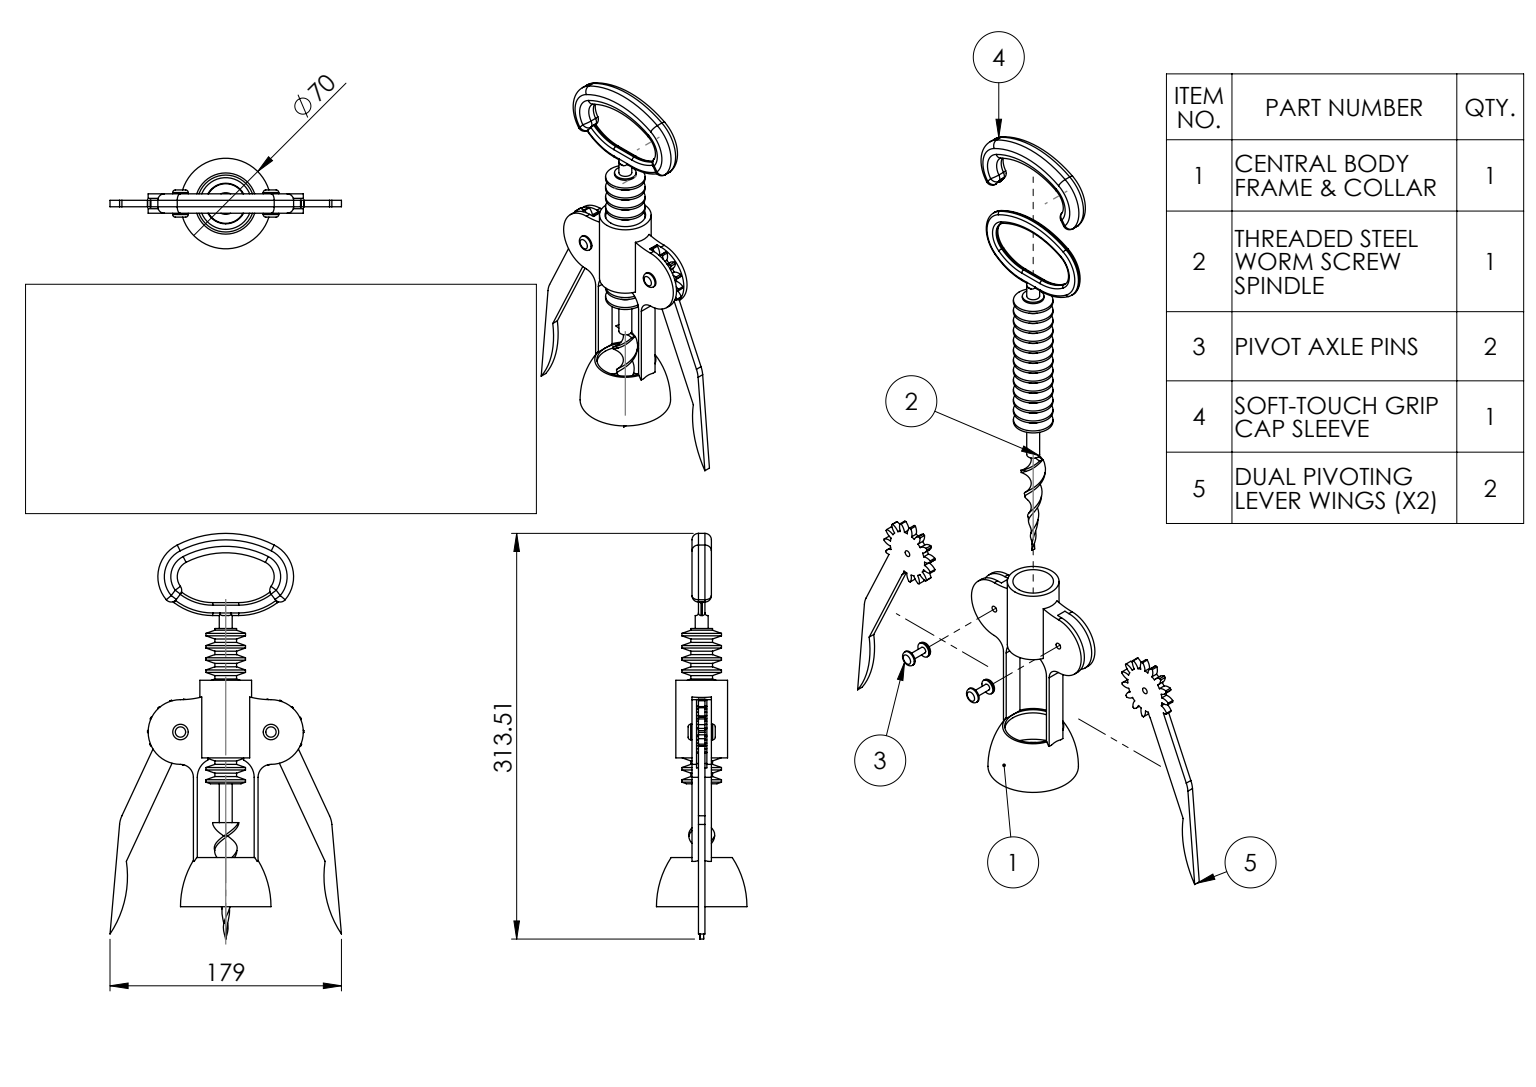
ISO-10303-21;
HEADER;
FILE_DESCRIPTION (('STEP AP214'),
    '1' );
FILE_NAME ('BR-824',
    '2026-10-08T14:03:35',
    ( '' ),
    ( '' ),
    'SwSTEP 2.0',
    'SolidWorks 2026',
    '' );
FILE_SCHEMA (( 'AUTOMOTIVE_DESIGN' ));
ENDSEC;

DATA;
#1 = EDGE_LOOP ( 'NONE', ( #6943, #8347, #5492, #144, #24, #10049, #6379, #1001, #2175, #10989 ) ) ;
#2 = ORIENTED_EDGE ( 'NONE', *, *, #10289, .F. ) ;
#3 = PRODUCT_RELATED_PRODUCT_CATEGORY ( 'part', '', ( #9019 ) ) ;
#4 = VECTOR ( 'NONE', #10867, 1000.000000000000000 ) ;
#5 = CIRCLE ( 'NONE', #8996, 5.999999999999998224 ) ;
#6 = DIRECTION ( 'NONE',  ( 0.9960067511297464593, -0.08927794634716622324, 3.401418580343279473E-17 ) ) ;
#7 = AXIS2_PLACEMENT_3D ( 'NONE', #7492, #359, #1391 ) ;
#8 = ORIENTED_EDGE ( 'NONE', *, *, #7820, .F. ) ;
#9 = ORIENTED_EDGE ( 'NONE', *, *, #2863, .F. ) ;
#10 = CYLINDRICAL_SURFACE ( 'NONE', #6059, 5.000000000000000000 ) ;
#11 = ORIENTED_EDGE ( 'NONE', *, *, #6966, .F. ) ;
#12 = DIRECTION ( 'NONE',  ( -1.000000000000000000, 0.000000000000000000, 0.000000000000000000 ) ) ;
#13 = CARTESIAN_POINT ( 'NONE',  ( 34.99999999999958789, 1.104930248025249758E-13, -2.499999999999999112 ) ) ;
#14 = DIRECTION ( 'NONE',  ( -1.000000000000000000, 0.000000000000000000, 0.000000000000000000 ) ) ;
#15 = CARTESIAN_POINT ( 'NONE',  ( 35.45454545454547457, 140.4866414850956460, 0.5000000000000000000 ) ) ;
#16 = CARTESIAN_POINT ( 'NONE',  ( -12.99553232110413248, 67.62342244460847951, -25.99106464220826851 ) ) ;
#17 = EDGE_CURVE ( 'NONE', #9929, #10530, #4223, .T. ) ;
#18 = VECTOR ( 'NONE', #6174, 1000.000000000000000 ) ;
#19 = CARTESIAN_POINT ( 'NONE',  ( 4.330127018922190985, 92.00000000000000000, -2.500000000000000000 ) ) ;
#20 = CARTESIAN_POINT ( 'NONE',  ( 10.69381717166375623, 25.55944687211528077, 0.000000000000000000 ) ) ;
#21 = ADVANCED_FACE ( 'NONE', ( #11217 ), #12542, .T. ) ;
#22 = ORIENTED_EDGE ( 'NONE', *, *, #10210, .T. ) ;
#23 = AXIS2_PLACEMENT_3D ( 'NONE', #10959, #4438, #5501 ) ;
#24 = ORIENTED_EDGE ( 'NONE', *, *, #1458, .F. ) ;
#25 = EDGE_LOOP ( 'NONE', ( #11281, #8827, #8911, #8959 ) ) ;
#26 = EDGE_CURVE ( 'NONE', #11146, #5183, #4908, .T. ) ;
#27 = EDGE_CURVE ( 'NONE', #5877, #10681, #5933, .T. ) ;
#28 = DIRECTION ( 'NONE',  ( -0.000000000000000000, -0.000000000000000000, -1.000000000000000000 ) ) ;
#29 = AXIS2_PLACEMENT_3D ( 'NONE', #13329, #9153, #677 ) ;
#30 = VERTEX_POINT ( 'NONE', #13473 ) ;
#31 = CARTESIAN_POINT ( 'NONE',  ( 25.00000000000000355, 120.0000000000000284, -0.5000000000000000000 ) ) ;
#32 = CARTESIAN_POINT ( 'NONE',  ( 8.259026987433399469, -87.08508809531834061, -4.189641850005036083 ) ) ;
#33 = CIRCLE ( 'NONE', #4726, 10.00000000000000178 ) ;
#34 = DIRECTION ( 'NONE',  ( 0.9960067511297463483, -0.08927794634716618161, 4.818676322152979407E-17 ) ) ;
#35 = CIRCLE ( 'NONE', #10337, 25.00000000000000711 ) ;
#36 = CARTESIAN_POINT ( 'NONE',  ( -12.99579180576517246, 64.08350967699263379, -3.310582014804570635E-15 ) ) ;
#37 = DIRECTION ( 'NONE',  ( -2.797435172181481150E-17, 1.000000000000000000, -1.765856845898762549E-18 ) ) ;
#38 = CARTESIAN_POINT ( 'NONE',  ( -4.250272934615508369, -76.81818181818270830, -9.136824450690360422 ) ) ;
#39 = DIRECTION ( 'NONE',  ( 1.000000000000000000, 0.000000000000000000, 0.000000000000000000 ) ) ;
#40 = DIRECTION ( 'NONE',  ( 1.000000000000000000, 8.163404592832038896E-16, 0.000000000000000000 ) ) ;
#41 = B_SPLINE_CURVE_WITH_KNOTS ( 'NONE', 3,
 ( #7096, #11371, #11645, #793, #10657, #9414, #8218, #1840, #4203, #6320, #13730, #12506, #2044, #8486, #3154, #2892, #3943, #7162, #10396, #1973, #13588, #10461, #11447, #12783, #5330, #6125, #4075, #12585, #8357, #859, #3030, #10593, #5066, #6254, #12653, #997, #11713, #7433, #2104, #9347, #5125, #1907, #13657, #4005, #8288, #6388, #5261, #1067, #2965, #7233, #7301, #11516, #11582, #3091, #9550, #6196, #8427, #10523, #931, #13858, #5196, #9484, #13791, #4141, #12715, #7359, #12055, #6584, #8618, #1398, #12856, #9746, #158, #7499, #6454, #13067, #1133, #3221, #9677, #5393, #292, #12926, #10918, #4547, #2170, #6728, #3289, #81, #6655, #1321, #7637, #10717, #10997, #7564, #11781, #2240, #8759, #3423, #4335, #11846, #8825, #2370, #2303, #8688, #6525, #10783, #4276, #9612 ),
 .UNSPECIFIED., .F., .F.,
 ( 4, 2, 2, 2, 2, 2, 2, 2, 2, 2, 2, 2, 2, 2, 2, 2, 2, 2, 2, 2, 2, 2, 2, 2, 2, 2, 2, 2, 2, 2, 2, 2, 2, 2, 2, 2, 2, 2, 2, 2, 2, 2, 2, 2, 2, 2, 2, 2, 2, 2, 2, 2, 2, 4 ),
 ( 1.115175723065530429E-16, 0.0007940898450324740008, 0.001588179690064836329, 0.003176359380129561202, 0.004764539070194286074, 0.006352718760259011381, 0.007940898450323734953, 0.009529078140388459392, 0.01111725783045318383, 0.01270543752051791001, 0.01588179690064744215, 0.01905815628077697083, 0.02223451566090650297, 0.02382269535097126731, 0.02541087504103603512, 0.02858723442116564359, 0.03017541411123044609, 0.03176359380129525206, 0.03493995318142493339, 0.03652813287148980875, 0.03811631256155468411, 0.04129267194168446953, 0.04288085163174937264, 0.04446903132181426188, 0.04764539070194404730, 0.04923357039200896429, 0.05082175008207386740, 0.05399810946220368751, 0.05717446884233351456, 0.05876264853239842462, 0.06035082822246332079, 0.06352718760259316866, 0.06511536729265808565, 0.06670354698272301652, 0.06829172667278794739, 0.06987990636285287827, 0.07305626574298272613, 0.07464444543304765700, 0.07623262512311257399, 0.07782080481317750487, 0.07940898450324243574, 0.08258534388337231136, 0.08417352357343724223, 0.08576170326350217310, 0.08734988295356710397, 0.08893806264363202096, 0.09211442202376185495, 0.09370260171382675807, 0.09529078140389167506, 0.09687896109395660593, 0.09846714078402152293, 0.1000553204740864260, 0.1008494103191188984, 0.1016435001641513708 ),
 .UNSPECIFIED. ) ;
#42 = VERTEX_POINT ( 'NONE', #3602 ) ;
#43 = EDGE_CURVE ( 'NONE', #8596, #8398, #2943, .T. ) ;
#44 = AXIS2_PLACEMENT_3D ( 'NONE', #13672, #4217, #12871 ) ;
#45 = AXIS2_PLACEMENT_3D ( 'NONE', #8376, #5215, #8445 ) ;
#46 = FACE_OUTER_BOUND ( 'NONE', #6458, .T. ) ;
#47 = EDGE_LOOP ( 'NONE', ( #4618, #2570, #12122, #10874, #7639, #5291, #7255 ) ) ;
#48 = ORIENTED_EDGE ( 'NONE', *, *, #13831, .T. ) ;
#49 = CARTESIAN_POINT ( 'NONE',  ( 2.406219558548489190E-16, -8.601520358636511432, 1.518905361043589440E-17 ) ) ;
#50 = ORIENTED_EDGE ( 'NONE', *, *, #9118, .T. ) ;
#51 = DIRECTION ( 'NONE',  ( 0.9960067511297463483, -0.08927794634716618161, 4.818676322152979407E-17 ) ) ;
#52 = DIRECTION ( 'NONE',  ( -2.797435172181481150E-17, 1.000000000000000000, -1.765856845898762549E-18 ) ) ;
#53 = CARTESIAN_POINT ( 'NONE',  ( 1.800977217354326365, -65.63636364725842043, 1.354836293522729163 ) ) ;
#54 = CIRCLE ( 'NONE', #4755, 69.24999999999975842 ) ;
#55 = B_SPLINE_CURVE_WITH_KNOTS ( 'NONE', 3,
 ( #12024, #7964, #3604, #11191, #2412, #1580, #5937, #3460, #13327, #5788, #331, #6692, #3526, #3678, #4586, #9152 ),
 .UNSPECIFIED., .F., .F.,
 ( 4, 2, 2, 2, 2, 2, 2, 4 ),
 ( 1.967444805616585729E-07, 0.0004077652619395022980, 0.0008153337793984429286, 0.001630470814316324190, 0.002038039331775264550, 0.002445607849234205343, 0.002853176366693145703, 0.003260744884152086496 ),
 .UNSPECIFIED. ) ;
#56 = FACE_OUTER_BOUND ( 'NONE', #8177, .T. ) ;
#57 = CARTESIAN_POINT ( 'NONE',  ( -8.385254915620292238, 24.75422479069652937, -16.77050983124059158 ) ) ;
#58 = CARTESIAN_POINT ( 'NONE',  ( -15.29705854078140348, -29.33764382806072746, 30.59411708156278920 ) ) ;
#59 = CARTESIAN_POINT ( 'NONE',  ( -2.079471018873752021E-15, 74.33491362204294717, -1.312648161087776599E-16 ) ) ;
#60 = DIRECTION ( 'NONE',  ( -1.000000000000000000, 0.000000000000000000, 0.000000000000000000 ) ) ;
#61 = EDGE_CURVE ( 'NONE', #7055, #3214, #4012, .T. ) ;
#62 = EDGE_LOOP ( 'NONE', ( #12490, #5333, #1562, #12326 ) ) ;
#63 = ORIENTED_EDGE ( 'NONE', *, *, #3775, .F. ) ;
#64 = CARTESIAN_POINT ( 'NONE',  ( -10.69381717166375800, 53.83378072214353693, -1.499740397452121781E-15 ) ) ;
#65 = LINE ( 'NONE', #1951, #2569 ) ;
#66 = CARTESIAN_POINT ( 'NONE',  ( 34.99999999999958789, 1.104930248025249758E-13, -2.499999999999999112 ) ) ;
#67 = CARTESIAN_POINT ( 'NONE',  ( -15.18222645069203125, -100.0000000000000000, -4.000000000000000000 ) ) ;
#68 = DIRECTION ( 'NONE',  ( -6.158143864569485777E-17, -2.736152283717910599E-16, 1.000000000000000000 ) ) ;
#69 = ORIENTED_EDGE ( 'NONE', *, *, #3097, .T. ) ;
#70 = ORIENTED_EDGE ( 'NONE', *, *, #7148, .F. ) ;
#71 = ADVANCED_FACE ( 'NONE', ( #7311 ), #13694, .F. ) ;
#72 = ORIENTED_EDGE ( 'NONE', *, *, #13139, .F. ) ;
#73 = ORIENTED_EDGE ( 'NONE', *, *, #707, .T. ) ;
#74 = ORIENTED_EDGE ( 'NONE', *, *, #8494, .F. ) ;
#75 = CARTESIAN_POINT ( 'NONE',  ( -34.99999999999999289, -97.00000000000000000, -7.500000000000000000 ) ) ;
#76 = AXIS2_PLACEMENT_3D ( 'NONE', #13638, #11239, #6171 ) ;
#77 = FACE_BOUND ( 'NONE', #7085, .T. ) ;
#78 = CARTESIAN_POINT ( 'NONE',  ( 0.3899450390716444614, -79.59552052770862929, -10.11716208056824762 ) ) ;
#79 = DIRECTION ( 'NONE',  ( -1.000000000000000000, 0.000000000000000000, 0.000000000000000000 ) ) ;
#80 = CARTESIAN_POINT ( 'NONE',  ( 3.915931169992960648, 90.55292468037850995, -3.111431273932147246 ) ) ;
#81 = CARTESIAN_POINT ( 'NONE',  ( -7.912770636739809405, -89.29698991853884138, 4.227864033747772865 ) ) ;
#82 = CARTESIAN_POINT ( 'NONE',  ( 25.00000000000001776, -100.0000000000000000, -5.046127144242417373 ) ) ;
#83 = EDGE_LOOP ( 'NONE', ( #9533, #5553, #4896, #10180 ) ) ;
#84 = ORIENTED_EDGE ( 'NONE', *, *, #10476, .F. ) ;
#85 = ORIENTED_EDGE ( 'NONE', *, *, #10554, .F. ) ;
#86 = AXIS2_PLACEMENT_3D ( 'NONE', #6886, #3650, #3573 ) ;
#87 = AXIS2_PLACEMENT_3D ( 'NONE', #13479, #2566, #7966 ) ;
#88 = ADVANCED_FACE ( 'NONE', ( #12662 ), #10538, .T. ) ;
#89 = DIRECTION ( 'NONE',  ( 6.158143864569485777E-17, 2.736152283717910599E-16, -1.000000000000000000 ) ) ;
#90 = EDGE_CURVE ( 'NONE', #3108, #8314, #5574, .T. ) ;
#91 = ORIENTED_EDGE ( 'NONE', *, *, #2062, .T. ) ;
#92 = DIRECTION ( 'NONE',  ( -0.8735848310779960046, 0.4866719047884612293, 9.637352644305955116E-17 ) ) ;
#93 = AXIS2_PLACEMENT_3D ( 'NONE', #1306, #12036, #9868 ) ;
#94 = DIRECTION ( 'NONE',  ( 0.000000000000000000, 0.000000000000000000, 1.000000000000000000 ) ) ;
#95 = CARTESIAN_POINT ( 'NONE',  ( 21.12690199240172007, 12.61198448588842425, -2.499999999999996447 ) ) ;
#96 = CARTESIAN_POINT ( 'NONE',  ( -2.905947830705728041, -133.0909090909398458, 2.158723819798283206 ) ) ;
#97 = CARTESIAN_POINT ( 'NONE',  ( -26.79177319725820894, -26.24642857144861807, -4.000000000000000000 ) ) ;
#98 = CARTESIAN_POINT ( 'NONE',  ( -60.00000000000001421, -4.286263797015736496E-15, 7.500000000000000000 ) ) ;
#99 = EDGE_CURVE ( 'NONE', #9883, #11270, #7176, .T. ) ;
#100 = CARTESIAN_POINT ( 'NONE',  ( 1.824130267506742786, -166.5454545852088017, -2.249022964541941061 ) ) ;
#101 = EDGE_CURVE ( 'NONE', #11832, #6555, #12065, .T. ) ;
#102 = CARTESIAN_POINT ( 'NONE',  ( -1.416598489609734557, -78.09090909090909349, -10.12631592825915838 ) ) ;
#103 = B_SPLINE_CURVE_WITH_KNOTS ( 'NONE', 3,
 ( #9323, #12223, #13300, #13225 ),
 .UNSPECIFIED., .F., .F.,
 ( 4, 4 ),
 ( 0.000000000000000000, 1.000000000000000000 ),
 .UNSPECIFIED. ) ;
#104 = CARTESIAN_POINT ( 'NONE',  ( 35.00000000000000000, 4.286263797015736496E-15, 7.500000000000000000 ) ) ;
#105 = LINE ( 'NONE', #1342, #981 ) ;
#106 = VECTOR ( 'NONE', #4632, 1000.000000000000000 ) ;
#107 = ORIENTED_EDGE ( 'NONE', *, *, #7623, .T. ) ;
#108 = CARTESIAN_POINT ( 'NONE',  ( 39.99999999999999289, 120.0000000000000142, -0.5000000000000000000 ) ) ;
#109 = CARTESIAN_POINT ( 'NONE',  ( 43.14708730495711819, 24.16350488746832781, 2.500000000000007105 ) ) ;
#110 = ORIENTED_EDGE ( 'NONE', *, *, #13403, .F. ) ;
#111 = CIRCLE ( 'NONE', #7943, 15.29705854078139460 ) ;
#112 = ADVANCED_FACE ( 'NONE', ( #12595 ), #4281, .T. ) ;
#113 = LINE ( 'NONE', #13095, #3464 ) ;
#114 = EDGE_CURVE ( 'NONE', #2716, #3638, #13476, .T. ) ;
#115 = DIRECTION ( 'NONE',  ( 0.000000000000000000, 0.000000000000000000, 1.000000000000000000 ) ) ;
#116 = ORIENTED_EDGE ( 'NONE', *, *, #6600, .T. ) ;
#117 = AXIS2_PLACEMENT_3D ( 'NONE', #10882, #1230, #12167 ) ;
#118 = CARTESIAN_POINT ( 'NONE',  ( 8.385254915620292238, 90.00000000000000000, 8.679704431140114636E-16 ) ) ;
#119 = CARTESIAN_POINT ( 'NONE',  ( -15.29705854078139637, 74.33491362204294717, -1.312648161087776599E-16 ) ) ;
#120 = CARTESIAN_POINT ( 'NONE',  ( -8.385254915620295790, 3.280056672672170492, 16.77050983124058448 ) ) ;
#121 = AXIS2_PLACEMENT_3D ( 'NONE', #813, #875, #8370 ) ;
#122 = EDGE_CURVE ( 'NONE', #8713, #9553, #6328, .T. ) ;
#123 = CARTESIAN_POINT ( 'NONE',  ( 35.00000000000009237, 91.25000000000046896, 4.000000000000000000 ) ) ;
#124 = EDGE_CURVE ( 'NONE', #4194, #10453, #1869, .T. ) ;
#125 = CARTESIAN_POINT ( 'NONE',  ( -12.99579180576517246, -20.73949187309215247, -1.518279536322449159E-15 ) ) ;
#126 = CARTESIAN_POINT ( 'NONE',  ( -8.385254915620294014, 12.70483462268159869, -2.089658196149648066E-15 ) ) ;
#127 = CYLINDRICAL_SURFACE ( 'NONE', #2611, 18.74900000001875000 ) ;
#128 = CYLINDRICAL_SURFACE ( 'NONE', #1187, 18.74900000001875000 ) ;
#129 = CARTESIAN_POINT ( 'NONE',  ( -35.00000000000000000, -4.286263797015736496E-15, 4.000000000000000000 ) ) ;
#130 = AXIS2_PLACEMENT_3D ( 'NONE', #4348, #7713, #2181 ) ;
#131 = VERTEX_POINT ( 'NONE', #11545 ) ;
#132 = AXIS2_PLACEMENT_3D ( 'NONE', #2558, #4657, #7593 ) ;
#133 = EDGE_CURVE ( 'NONE', #3737, #3625, #5810, .T. ) ;
#134 = ADVANCED_FACE ( 'NONE', ( #1030, #12741 ), #7261, .F. ) ;
#135 = ORIENTED_EDGE ( 'NONE', *, *, #9456, .T. ) ;
#136 = ORIENTED_EDGE ( 'NONE', *, *, #744, .F. ) ;
#137 = AXIS2_PLACEMENT_3D ( 'NONE', #11805, #13167, #2478 ) ;
#138 = CARTESIAN_POINT ( 'NONE',  ( -49.99999999999999289, 120.0000000000000142, -0.5000000000000000000 ) ) ;
#139 = EDGE_CURVE ( 'NONE', #6890, #1913, #9510, .T. ) ;
#140 = FACE_OUTER_BOUND ( 'NONE', #958, .T. ) ;
#141 = VECTOR ( 'NONE', #5529, 1000.000000000000000 ) ;
#142 = CARTESIAN_POINT ( 'NONE',  ( -35.00000000000000000, 25.00000000000000000, -4.000000000000000000 ) ) ;
#143 = DIRECTION ( 'NONE',  ( -2.797435172181481150E-17, 1.000000000000000000, -1.765856845898762549E-18 ) ) ;
#144 = ORIENTED_EDGE ( 'NONE', *, *, #11064, .F. ) ;
#145 = EDGE_LOOP ( 'NONE', ( #4394, #1634, #10776, #9029 ) ) ;
#146 = AXIS2_PLACEMENT_3D ( 'NONE', #3923, #12417, #8205 ) ;
#147 = CIRCLE ( 'NONE', #5069, 5.000000000000000000 ) ;
#148 = ORIENTED_EDGE ( 'NONE', *, *, #400, .T. ) ;
#149 = VERTEX_POINT ( 'NONE', #5637 ) ;
#150 = CARTESIAN_POINT ( 'NONE',  ( 15.29705854078138927, 55.48535772202409078, 1.773704474924340737E-15 ) ) ;
#151 = ORIENTED_EDGE ( 'NONE', *, *, #13444, .T. ) ;
#152 = DIRECTION ( 'NONE',  ( 1.000000000000000000, 0.000000000000000000, 0.000000000000000000 ) ) ;
#153 = CARTESIAN_POINT ( 'NONE',  ( 43.29712336220986657, 19.44704974301885159, -2.499999999999993783 ) ) ;
#154 = AXIS2_PLACEMENT_3D ( 'NONE', #13891, #2740, #9326 ) ;
#155 =( LENGTH_UNIT ( ) NAMED_UNIT ( * ) SI_UNIT ( .MILLI., .METRE. ) );
#156 = DIRECTION ( 'NONE',  ( -2.797435172181481150E-17, 1.000000000000000000, -1.765856845898762549E-18 ) ) ;
#157 = DIRECTION ( 'NONE',  ( -0.6001121574638169642, 0.7999158696163758409, 1.927470528861191270E-16 ) ) ;
#158 = CARTESIAN_POINT ( 'NONE',  ( -5.529376117763302290, -98.63915323273988633, -5.578400940830572807 ) ) ;
#159 = B_SPLINE_CURVE_WITH_KNOTS ( 'NONE', 3,
 ( #12320, #4952, #9234, #13548 ),
 .UNSPECIFIED., .F., .F.,
 ( 4, 4 ),
 ( 0.000000000000000000, 1.000000000000000000 ),
 .UNSPECIFIED. ) ;
#160 = CYLINDRICAL_SURFACE ( 'NONE', #3931, 25.50000000002549783 ) ;
#161 = ORIENTED_EDGE ( 'NONE', *, *, #4188, .T. ) ;
#162 = ORIENTED_EDGE ( 'NONE', *, *, #8775, .F. ) ;
#163 = ORIENTED_EDGE ( 'NONE', *, *, #556, .F. ) ;
#164 = CIRCLE ( 'NONE', #12478, 50.00000000000001421 ) ;
#165 = FACE_OUTER_BOUND ( 'NONE', #5586, .T. ) ;
#166 = CARTESIAN_POINT ( 'NONE',  ( 31.81818181818183433, 133.3608531424536920, 2.500000000000000000 ) ) ;
#167 = ORIENTED_EDGE ( 'NONE', *, *, #10705, .F. ) ;
#168 = CYLINDRICAL_SURFACE ( 'NONE', #12862, 25.50000000002549783 ) ;
#169 = CARTESIAN_POINT ( 'NONE',  ( -15.29705854078138927, 19.67281349139174296, -3.473937238186366113E-17 ) ) ;
#170 = DIRECTION ( 'NONE',  ( -6.158143864569485777E-17, -2.736152283717910599E-16, 1.000000000000000000 ) ) ;
#171 = DIRECTION ( 'NONE',  ( 0.000000000000000000, 0.000000000000000000, 1.000000000000000000 ) ) ;
#172 = CYLINDRICAL_SURFACE ( 'NONE', #13260, 80.00000000000001421 ) ;
#173 = CARTESIAN_POINT ( 'NONE',  ( -9.456627357064087747, -73.18181818181821541, -3.908318357316046487 ) ) ;
#174 = CYLINDRICAL_SURFACE ( 'NONE', #4487, 2.500000000000002220 ) ;
#175 = CARTESIAN_POINT ( 'NONE',  ( 53.63671053572210923, -2.048907369402451106, 2.500000000000000444 ) ) ;
#176 = ADVANCED_FACE ( 'NONE', ( #6620 ), #9921, .T. ) ;
#177 = ORIENTED_EDGE ( 'NONE', *, *, #6787, .T. ) ;
#178 = DIRECTION ( 'NONE',  ( 1.000000000000000000, 0.000000000000000000, 0.000000000000000000 ) ) ;
#179 = ORIENTED_EDGE ( 'NONE', *, *, #7625, .T. ) ;
#180 = CARTESIAN_POINT ( 'NONE',  ( -2.517691654963332357E-15, 90.00000000000000000, -1.589271161308885878E-16 ) ) ;
#181 = DIRECTION ( 'NONE',  ( -0.000000000000000000, -0.000000000000000000, -1.000000000000000000 ) ) ;
#182 = VERTEX_POINT ( 'NONE', #256 ) ;
#183 = CARTESIAN_POINT ( 'NONE',  ( -12.99579180576516535, 7.534841976936128560, -1.618136388307047266E-15 ) ) ;
#184 = CARTESIAN_POINT ( 'NONE',  ( -35.00000000000012079, 91.25000000000045475, -7.500000000000000000 ) ) ;
#185 = CARTESIAN_POINT ( 'NONE',  ( 12.99579180576516713, 73.50828762700209040, 0.000000000000000000 ) ) ;
#186 = CARTESIAN_POINT ( 'NONE',  ( 41.86252833142972918, 24.55922850786694056, 2.500000000000007105 ) ) ;
#187 = DIRECTION ( 'NONE',  ( -1.000000000000000000, 0.000000000000000000, 0.000000000000000000 ) ) ;
#188 = FACE_OUTER_BOUND ( 'NONE', #11939, .T. ) ;
#189 = DIRECTION ( 'NONE',  ( -6.158143864569485777E-17, -2.736152283717910599E-16, 1.000000000000000000 ) ) ;
#190 = EDGE_CURVE ( 'NONE', #2348, #11393, #10077, .T. ) ;
#191 = DIRECTION ( 'NONE',  ( -2.797435172181481150E-17, 1.000000000000000000, -1.765856845898762549E-18 ) ) ;
#192 = ADVANCED_FACE ( 'NONE', ( #6688 ), #1879, .T. ) ;
#193 = ADVANCED_FACE ( 'NONE', ( #9782 ), #3762, .T. ) ;
#194 = CARTESIAN_POINT ( 'NONE',  ( 35.00000000000000000, 4.286263797015736496E-15, 4.000000000000000000 ) ) ;
#195 = EDGE_LOOP ( 'NONE', ( #3953, #4577 ) ) ;
#196 = CARTESIAN_POINT ( 'NONE',  ( 0.000000000000000000, 71.01020514433645303, 7.500000000000000000 ) ) ;
#197 = ADVANCED_FACE ( 'NONE', ( #5497 ), #1357, .T. ) ;
#198 = ADVANCED_FACE ( 'NONE', ( #8588 ), #2424, .T. ) ;
#199 = AXIS2_PLACEMENT_3D ( 'NONE', #10505, #5245, #13714 ) ;
#200 = ORIENTED_EDGE ( 'NONE', *, *, #12255, .T. ) ;
#201 = AXIS2_PLACEMENT_3D ( 'NONE', #5042, #6172, #12757 ) ;
#202 = ORIENTED_EDGE ( 'NONE', *, *, #10624, .T. ) ;
#203 = CARTESIAN_POINT ( 'NONE',  ( 80.29381926039658879, -64.72749139719506672, -2.500000000000000000 ) ) ;
#204 = FACE_OUTER_BOUND ( 'NONE', #4519, .T. ) ;
#205 = PLANE ( 'NONE',  #6332 ) ;
#206 = AXIS2_PLACEMENT_3D ( 'NONE', #6163, #5168, #5231 ) ;
#207 = EDGE_CURVE ( 'NONE', #13779, #9777, #1115, .T. ) ;
#208 = DIRECTION ( 'NONE',  ( 1.000000000000000000, 0.000000000000000000, -0.000000000000000000 ) ) ;
#209 = EDGE_LOOP ( 'NONE', ( #5485, #10650, #4189, #10104 ) ) ;
#210 = ORIENTED_EDGE ( 'NONE', *, *, #10551, .T. ) ;
#211 = EDGE_CURVE ( 'NONE', #2222, #2825, #5653, .T. ) ;
#212 = CARTESIAN_POINT ( 'NONE',  ( -13.79311422413708499, -100.0000000000000000, 7.500000000000000000 ) ) ;
#213 = EDGE_LOOP ( 'NONE', ( #12461, #12603, #11855, #6788 ) ) ;
#214 = VERTEX_POINT ( 'NONE', #5795 ) ;
#215 = DIRECTION ( 'NONE',  ( -2.797435172181481150E-17, 1.000000000000000000, -1.765856845898762549E-18 ) ) ;
#216 = ORIENTED_EDGE ( 'NONE', *, *, #1663, .T. ) ;
#217 = CARTESIAN_POINT ( 'NONE',  ( -1.868594470333698657E-15, 66.79670324143890525, -1.179534157023628988E-16 ) ) ;
#218 = DIRECTION ( 'NONE',  ( -0.000000000000000000, -0.000000000000000000, -1.000000000000000000 ) ) ;
#219 = CYLINDRICAL_SURFACE ( 'NONE', #7081, 8.385254915620292238 ) ;
#220 = DIRECTION ( 'NONE',  ( 0.1928999275155749149, 0.9812184353977894125, 2.775705599192072226E-16 ) ) ;
#221 = CARTESIAN_POINT ( 'NONE',  ( -15.29705854078139282, -29.33764382806072746, -30.59411708156279630 ) ) ;
#222 = DIRECTION ( 'NONE',  ( 6.158143864569485777E-17, 2.736152283717910599E-16, -1.000000000000000000 ) ) ;
#223 = EDGE_LOOP ( 'NONE', ( #1388, #322, #1636, #10853 ) ) ;
#224 = AXIS2_PLACEMENT_3D ( 'NONE', #10271, #2564, #8106 ) ;
#225 = ORIENTED_EDGE ( 'NONE', *, *, #6865, .T. ) ;
#226 = ORIENTED_EDGE ( 'NONE', *, *, #7270, .T. ) ;
#227 = AXIS2_PLACEMENT_3D ( 'NONE', #6286, #961, #5222 ) ;
#228 = FACE_OUTER_BOUND ( 'NONE', #3050, .T. ) ;
#229 = CARTESIAN_POINT ( 'NONE',  ( -0.9875499244693202172, -80.00464164737402939, 10.06307371418729701 ) ) ;
#230 = ORIENTED_EDGE ( 'NONE', *, *, #3262, .F. ) ;
#231 = DIRECTION ( 'NONE',  ( -1.224646799147353207E-16, 1.000000000000000000, 0.000000000000000000 ) ) ;
#232 = CARTESIAN_POINT ( 'NONE',  ( -25.00000000000000355, 120.0000000000000284, 0.5000000000000000000 ) ) ;
#233 = CARTESIAN_POINT ( 'NONE',  ( -15.29705854078139637, 0.8232575913728885642, -1.453755053663958216E-18 ) ) ;
#234 = DIRECTION ( 'NONE',  ( -1.000000000000000000, 0.000000000000000000, 0.000000000000000000 ) ) ;
#235 = CARTESIAN_POINT ( 'NONE',  ( -2.866821506922881722E-16, 10.24803554138234496, -1.809656371776380929E-17 ) ) ;
#236 = CARTESIAN_POINT ( 'NONE',  ( 1.713057075396043238, -163.8787878899150030, 2.641018403436653728 ) ) ;
#237 = VECTOR ( 'NONE', #1930, 1000.000000000000000 ) ;
#238 = CARTESIAN_POINT ( 'NONE',  ( 15.29705854078138927, 46.06057977201469100, 1.790347283588440388E-15 ) ) ;
#239 = CIRCLE ( 'NONE', #906, 9.000000000008999024 ) ;
#240 = CARTESIAN_POINT ( 'NONE',  ( 18.54049621773915746, -20.00000000000000000, -7.500000000000000000 ) ) ;
#241 = FILL_AREA_STYLE ('',( #9833 ) ) ;
#242 = ORIENTED_EDGE ( 'NONE', *, *, #7205, .T. ) ;
#243 = CYLINDRICAL_SURFACE ( 'NONE', #12092, 8.385254915620295790 ) ;
#244 = CARTESIAN_POINT ( 'NONE',  ( 0.4999999999999966693, 79.99058638175036151, -2.499999999999982236 ) ) ;
#245 = AXIS2_PLACEMENT_3D ( 'NONE', #10275, #9294, #13478 ) ;
#246 = ORIENTED_EDGE ( 'NONE', *, *, #1045, .F. ) ;
#247 = CIRCLE ( 'NONE', #2028, 15.29705854078138572 ) ;
#248 = AXIS2_PLACEMENT_3D ( 'NONE', #3744, #8028, #12308 ) ;
#249 = DIRECTION ( 'NONE',  ( 0.000000000000000000, -1.000000000000000000, 0.000000000000000000 ) ) ;
#250 = CARTESIAN_POINT ( 'NONE',  ( 36.36363636363638108, 142.2680885707561629, 2.500000000000000000 ) ) ;
#251 = ORIENTED_EDGE ( 'NONE', *, *, #10047, .F. ) ;
#252 = DIRECTION ( 'NONE',  ( -2.797435172181481150E-17, 1.000000000000000000, -1.765856845898762549E-18 ) ) ;
#253 = ORIENTED_EDGE ( 'NONE', *, *, #309, .F. ) ;
#254 = CARTESIAN_POINT ( 'NONE',  ( 51.25836974494252019, 19.64472991003004054, 6.505213034913026604E-15 ) ) ;
#255 = EDGE_CURVE ( 'NONE', #10763, #2744, #8961, .T. ) ;
#256 = CARTESIAN_POINT ( 'NONE',  ( 23.90723890023449627, -15.11541108221136476, -2.500000000000003553 ) ) ;
#257 = DIRECTION ( 'NONE',  ( -0.000000000000000000, -0.000000000000000000, 1.000000000000000000 ) ) ;
#258 = AXIS2_PLACEMENT_3D ( 'NONE', #3303, #12076, #6668 ) ;
#259 = CARTESIAN_POINT ( 'NONE',  ( -12.99579180576516713, -1.889935973073298525, -1.584850770978847568E-15 ) ) ;
#260 = DIRECTION ( 'NONE',  ( 0.000000000000000000, 0.000000000000000000, 1.000000000000000000 ) ) ;
#261 = FACE_OUTER_BOUND ( 'NONE', #11503, .T. ) ;
#262 = DIRECTION ( 'NONE',  ( -1.000000000000000000, -5.171946152600902986E-17, 0.000000000000000000 ) ) ;
#263 = AXIS2_PLACEMENT_3D ( 'NONE', #6259, #865, #11653 ) ;
#264 = B_SPLINE_CURVE_WITH_KNOTS ( 'NONE', 3,
 ( #3142, #782, #3995, #11363 ),
 .UNSPECIFIED., .F., .F.,
 ( 4, 4 ),
 ( 0.000000000000000000, 1.000000000000000000 ),
 .UNSPECIFIED. ) ;
#265 = ORIENTED_EDGE ( 'NONE', *, *, #867, .T. ) ;
#266 = ORIENTED_EDGE ( 'NONE', *, *, #11663, .F. ) ;
#267 = LINE ( 'NONE', #5318, #5455 ) ;
#268 = CIRCLE ( 'NONE', #8110, 14.99999999999998934 ) ;
#269 = EDGE_CURVE ( 'NONE', #10258, #13109, #10073, .T. ) ;
#270 = PRODUCT_CONTEXT ( 'NONE', #3147, 'mechanical' ) ;
#271 = EDGE_CURVE ( 'NONE', #8931, #12042, #8495, .T. ) ;
#272 = ORIENTED_EDGE ( 'NONE', *, *, #8857, .F. ) ;
#273 = CARTESIAN_POINT ( 'NONE',  ( 35.22727272727274794, 140.0412797136805523, 2.499999999999999556 ) ) ;
#274 = CARTESIAN_POINT ( 'NONE',  ( -12.99553232110413781, 39.34908859458022334, -1.730463420974848368E-15 ) ) ;
#275 = EDGE_CURVE ( 'NONE', #4145, #2418, #159, .T. ) ;
#276 = ADVANCED_FACE ( 'NONE', ( #3756, #3111 ), #953, .F. ) ;
#277 = DIRECTION ( 'NONE',  ( -1.000000000000000000, 0.000000000000000000, 0.000000000000000000 ) ) ;
#278 = CARTESIAN_POINT ( 'NONE',  ( 10.69346802281034492, 11.89973432371241380, 2.619144277183853160E-15 ) ) ;
#279 = ORIENTED_EDGE ( 'NONE', *, *, #778, .T. ) ;
#280 = AXIS2_PLACEMENT_3D ( 'NONE', #8444, #12670, #13811 ) ;
#281 = EDGE_LOOP ( 'NONE', ( #6165, #11619, #12587 ) ) ;
#282 = CARTESIAN_POINT ( 'NONE',  ( -25.00000000000000355, 120.0000000000000284, -0.5000000000000000000 ) ) ;
#283 = VERTEX_POINT ( 'NONE', #6077 ) ;
#284 = CARTESIAN_POINT ( 'NONE',  ( -15.29705854078138394, 76.22148119144830503, -30.59411708156277854 ) ) ;
#285 = ORIENTED_EDGE ( 'NONE', *, *, #8017, .F. ) ;
#286 = DIRECTION ( 'NONE',  ( 0.1234677578012386701, 0.000000000000000000, -0.9923485843107424653 ) ) ;
#287 = CARTESIAN_POINT ( 'NONE',  ( 5.570495138619319060E-16, -19.91286587805129926, 3.516327053222078456E-17 ) ) ;
#288 = FILL_AREA_STYLE_COLOUR ( '', #11871 ) ;
#289 = EDGE_CURVE ( 'NONE', #6878, #1278, #2220, .T. ) ;
#290 = DIRECTION ( 'NONE',  ( 0.000000000000000000, 0.000000000000000000, -1.000000000000000000 ) ) ;
#291 = CARTESIAN_POINT ( 'NONE',  ( 4.317896099768522511, 91.66241202089436513, -2.521541801375117853 ) ) ;
#292 = CARTESIAN_POINT ( 'NONE',  ( -8.281054986618348934, -94.04345070189340561, -1.330912282001587954 ) ) ;
#293 = CARTESIAN_POINT ( 'NONE',  ( -15.29705854078139282, 90.00000000000000000, -1.589271161308885878E-16 ) ) ;
#294 = ORIENTED_EDGE ( 'NONE', *, *, #6674, .T. ) ;
#295 = CIRCLE ( 'NONE', #9689, 77.99999999999997158 ) ;
#296 = EDGE_LOOP ( 'NONE', ( #12676, #4447, #755, #3036 ) ) ;
#297 = VERTEX_POINT ( 'NONE', #11394 ) ;
#298 = AXIS2_PLACEMENT_3D ( 'NONE', #1298, #13105, #6426 ) ;
#299 = CARTESIAN_POINT ( 'NONE',  ( -7.887411832334696449, -93.14649341443603703, -3.265743713357469602 ) ) ;
#300 = CARTESIAN_POINT ( 'NONE',  ( -3.915931169992964200, 90.55292468037848153, 3.111431273932144581 ) ) ;
#301 = EDGE_CURVE ( 'NONE', #2246, #7494, #13812, .T. ) ;
#302 = LINE ( 'NONE', #4555, #8293 ) ;
#303 = EDGE_LOOP ( 'NONE', ( #1188, #1446, #12340 ) ) ;
#304 = CARTESIAN_POINT ( 'NONE',  ( -12.99579180576516713, -1.889935973073298525, -1.584850770978847568E-15 ) ) ;
#305 = CARTESIAN_POINT ( 'NONE',  ( -12.99579180576516713, 35.80917582696438473, -1.717993240291646161E-15 ) ) ;
#306 = CARTESIAN_POINT ( 'NONE',  ( 15.29705854078139460, -8.601520358636511432, 1.890204135573040269E-15 ) ) ;
#307 = CARTESIAN_POINT ( 'NONE',  ( 25.00000000000000355, 120.0000000000000284, 0.5000000000000000000 ) ) ;
#308 = CARTESIAN_POINT ( 'NONE',  ( -10.11144051725924520, -69.99977036137985920, 0.2534939247371171822 ) ) ;
#309 = EDGE_CURVE ( 'NONE', #10920, #8708, #4021, .T. ) ;
#310 = CARTESIAN_POINT ( 'NONE',  ( -2.517691654963332357E-15, 90.00000000000000000, -1.589271161308885878E-16 ) ) ;
#311 = CARTESIAN_POINT ( 'NONE',  ( -15.29705854078139460, -18.02629830864593785, -1.809685653284690613E-15 ) ) ;
#312 = DIRECTION ( 'NONE',  ( -2.797435172181481150E-17, 1.000000000000000000, -1.765856845898762549E-18 ) ) ;
#313 = VECTOR ( 'NONE', #2315, 1000.000000000000000 ) ;
#314 = ORIENTED_EDGE ( 'NONE', *, *, #9696, .T. ) ;
#315 = ORIENTED_EDGE ( 'NONE', *, *, #6674, .F. ) ;
#316 = AXIS2_PLACEMENT_3D ( 'NONE', #6986, #3754, #479 ) ;
#317 = DIRECTION ( 'NONE',  ( -6.158143864569485777E-17, -2.736152283717910599E-16, 1.000000000000000000 ) ) ;
#318 = CARTESIAN_POINT ( 'NONE',  ( -15.29705854078138927, 74.33491362204296138, -30.59411708156278564 ) ) ;
#319 = CARTESIAN_POINT ( 'NONE',  ( 52.26118412238654543, 18.64354822589355365, 2.500000000000006217 ) ) ;
#320 = CARTESIAN_POINT ( 'NONE',  ( -4.288313376222440694E-16, 15.32944684068712782, -2.706960864746847057E-17 ) ) ;
#321 = EDGE_LOOP ( 'NONE', ( #4799, #6179, #1264, #10017 ) ) ;
#322 = ORIENTED_EDGE ( 'NONE', *, *, #4730, .F. ) ;
#323 = CARTESIAN_POINT ( 'NONE',  ( 35.45454545454547457, 140.4866414850956744, -0.5000000000000000000 ) ) ;
#324 = ORIENTED_EDGE ( 'NONE', *, *, #2209, .F. ) ;
#325 = CARTESIAN_POINT ( 'NONE',  ( -22.42156014662057473, -97.00000000000000000, -7.500000000000000000 ) ) ;
#326 = CARTESIAN_POINT ( 'NONE',  ( -15.29705854078139460, 27.21102387199583461, 30.59411708156277854 ) ) ;
#327 = CARTESIAN_POINT ( 'NONE',  ( 13.79311422413708499, -20.00000000000000355, 7.500000000000000000 ) ) ;
#328 = AXIS2_PLACEMENT_3D ( 'NONE', #13578, #6044, #1960 ) ;
#329 = CARTESIAN_POINT ( 'NONE',  ( -25.00000000000000355, 120.0000000000000284, -0.5000000000000000000 ) ) ;
#330 = DIRECTION ( 'NONE',  ( -0.4545454545454531425, -0.8907235428302472391, 0.000000000000000000 ) ) ;
#331 = CARTESIAN_POINT ( 'NONE',  ( -39.64259366921353944, 101.1295926276828396, -2.298140577494256931 ) ) ;
#332 = CARTESIAN_POINT ( 'NONE',  ( -19.99988111993867079, 26.72048013816596779, 0.6453928856983819351 ) ) ;
#333 = CARTESIAN_POINT ( 'NONE',  ( -35.00000000000000000, -4.286263797015736496E-15, 7.500000000000000000 ) ) ;
#334 = DIRECTION ( 'NONE',  ( -0.000000000000000000, -0.000000000000000000, -1.000000000000000000 ) ) ;
#335 = CARTESIAN_POINT ( 'NONE',  ( 14.79219767565757770, 6.218900627562692129, -2.499999999999999112 ) ) ;
#336 = ORIENTED_EDGE ( 'NONE', *, *, #5229, .T. ) ;
#337 = FACE_OUTER_BOUND ( 'NONE', #1428, .T. ) ;
#338 = ORIENTED_EDGE ( 'NONE', *, *, #5869, .F. ) ;
#339 = CIRCLE ( 'NONE', #9953, 18.74900000001874645 ) ;
#340 = ORIENTED_EDGE ( 'NONE', *, *, #4739, .T. ) ;
#341 = DIRECTION ( 'NONE',  ( 1.000000000000000000, 0.000000000000000000, 0.000000000000000000 ) ) ;
#342 = APPLICATION_PROTOCOL_DEFINITION ( 'draft international standard', 'automotive_design', 1998, #6296 ) ;
#343 = ORIENTED_EDGE ( 'NONE', *, *, #10693, .T. ) ;
#344 = CARTESIAN_POINT ( 'NONE',  ( 22.31663499682298735, 16.91633092580596198, -2.499999999999995559 ) ) ;
#345 = DIRECTION ( 'NONE',  ( -0.000000000000000000, -0.000000000000000000, -1.000000000000000000 ) ) ;
#346 = CARTESIAN_POINT ( 'NONE',  ( 1.119237408740483668E-15, -40.00941361824963849, 7.065089693818137167E-17 ) ) ;
#347 = AXIS2_PLACEMENT_3D ( 'NONE', #5420, #4428, #2399 ) ;
#348 = CARTESIAN_POINT ( 'NONE',  ( -37.50000000000000711, -4.286263797015736496E-15, 7.500000000000000000 ) ) ;
#349 = DIRECTION ( 'NONE',  ( -0.1234677578008764876, 2.460994371251751031E-11, 0.9923485843107875404 ) ) ;
#350 = AXIS2_PLACEMENT_3D ( 'NONE', #10266, #11321, #5862 ) ;
#351 = ORIENTED_EDGE ( 'NONE', *, *, #9753, .F. ) ;
#352 = EDGE_CURVE ( 'NONE', #2949, #3802, #8059, .T. ) ;
#353 = ORIENTED_EDGE ( 'NONE', *, *, #1966, .F. ) ;
#354 = EDGE_CURVE ( 'NONE', #717, #1714, #10955, .T. ) ;
#355 = ORIENTED_EDGE ( 'NONE', *, *, #4560, .T. ) ;
#356 = CARTESIAN_POINT ( 'NONE',  ( 8.385254915620295790, -24.99427717735608212, 1.068716529980328740E-15 ) ) ;
#357 = VERTEX_POINT ( 'NONE', #882 ) ;
#358 = EDGE_LOOP ( 'NONE', ( #9572, #5128, #4628, #12509 ) ) ;
#359 = DIRECTION ( 'NONE',  ( -2.797435172181481150E-17, 1.000000000000000000, -1.765856845898762549E-18 ) ) ;
#360 = MECHANICAL_DESIGN_GEOMETRIC_PRESENTATION_REPRESENTATION (  '', ( #8623 ), #10638 ) ;
#361 = CARTESIAN_POINT ( 'NONE',  ( 89.49979561504950709, -156.1132911148542917, 2.500000000000000000 ) ) ;
#362 = AXIS2_PLACEMENT_3D ( 'NONE', #3358, #4277, #12857 ) ;
#363 = DIRECTION ( 'NONE',  ( -6.158143864569485777E-17, -2.736152283717910599E-16, 1.000000000000000000 ) ) ;
#364 = CARTESIAN_POINT ( 'NONE',  ( 19.96844336951937748, 26.72776445485856911, -1.294012040295340782 ) ) ;
#365 = DIRECTION ( 'NONE',  ( 0.000000000000000000, 0.000000000000000000, 1.000000000000000000 ) ) ;
#366 = CARTESIAN_POINT ( 'NONE',  ( 15.29705854078138749, 57.37192529142945574, 3.746698755667522411E-15 ) ) ;
#367 = ORIENTED_EDGE ( 'NONE', *, *, #12940, .T. ) ;
#368 = EDGE_CURVE ( 'NONE', #4551, #8182, #6045, .T. ) ;
#369 = VERTEX_POINT ( 'NONE', #1786 ) ;
#370 = VECTOR ( 'NONE', #9228, 1000.000000000000000 ) ;
#371 = CARTESIAN_POINT ( 'NONE',  ( -7.177581306179082077, -94.18858243930635865, -4.303391048795623064 ) ) ;
#372 = DIRECTION ( 'NONE',  ( -1.000000000000000000, 0.000000000000000000, 0.000000000000000000 ) ) ;
#373 = ADVANCED_FACE ( 'NONE', ( #13878 ), #5017, .F. ) ;
#374 =( BOUNDED_SURFACE ( )  B_SPLINE_SURFACE ( 3, 3, ( 
 ( #3071, #10573, #976, #9525 ),
 ( #7481, #12037, #5514, #9661 ),
 ( #6639, #11762, #5441, #8537 ),
 ( #7615, #5310, #2217, #8808 ) ),
 .UNSPECIFIED., .F., .F., .F. ) 
 B_SPLINE_SURFACE_WITH_KNOTS ( ( 4, 4 ),
 ( 4, 4 ),
 ( 0.000000000000000000, 1.000000000000000000 ),
 ( 0.000000000000000000, 1.000000000000000000 ),
 .UNSPECIFIED. ) 
 GEOMETRIC_REPRESENTATION_ITEM ( )  RATIONAL_B_SPLINE_SURFACE ( (
 ( 1.000000000000000000, 0.3333333333333334259, 0.3333333333333334259, 1.000000000000000000),
 ( 1.000000000000000000, 0.3333333333333334259, 0.3333333333333334259, 1.000000000000000000),
 ( 1.000000000000000000, 0.3333333333333334259, 0.3333333333333334259, 1.000000000000000000),
 ( 1.000000000000000000, 0.3333333333333334259, 0.3333333333333334259, 1.000000000000000000) ) ) 
 REPRESENTATION_ITEM ( '' )  SURFACE ( )  );
#375 = EDGE_CURVE ( 'NONE', #7425, #1069, #7596, .T. ) ;
#376 = ORIENTED_EDGE ( 'NONE', *, *, #1897, .T. ) ;
#377 = DIRECTION ( 'NONE',  ( 0.000000000000000000, 0.000000000000000000, 1.000000000000000000 ) ) ;
#378 = DIRECTION ( 'NONE',  ( -6.158143864569485777E-17, -2.736152283717910599E-16, 1.000000000000000000 ) ) ;
#379 = EDGE_LOOP ( 'NONE', ( #6863, #5264, #11175, #13440 ) ) ;
#380 = DIRECTION ( 'NONE',  ( -2.797435172181481150E-17, 1.000000000000000000, -1.765856845898762549E-18 ) ) ;
#381 = AXIS2_PLACEMENT_3D ( 'NONE', #9717, #9650, #7739 ) ;
#382 = DIRECTION ( 'NONE',  ( 1.000000000000000000, 0.000000000000000000, 0.000000000000000000 ) ) ;
#383 = CARTESIAN_POINT ( 'NONE',  ( 8.385254915620292238, 59.82872437272870769, -16.77050983124058092 ) ) ;
#384 = LINE ( 'NONE', #7781, #5223 ) ;
#385 = CARTESIAN_POINT ( 'NONE',  ( -2.134167523385911647, -102.5454545454534099, -7.554873526040499776 ) ) ;
#386 = CARTESIAN_POINT ( 'NONE',  ( -15.29705854078139282, 46.06057977201469100, -8.133639011647813827E-17 ) ) ;
#387 = CARTESIAN_POINT ( 'NONE',  ( 15.29705854078139815, -18.02629830864593785, -30.59411708156277854 ) ) ;
#388 = CARTESIAN_POINT ( 'NONE',  ( 7.181435285653160250, -97.41991341991979425, 5.065585088379008560 ) ) ;
#389 = CARTESIAN_POINT ( 'NONE',  ( 37.49001687782395464, -0.2231948658678056807, 2.500000000000000000 ) ) ;
#390 = DIRECTION ( 'NONE',  ( 0.9960067511297464593, -0.08927794634716622324, 3.401418580343279473E-17 ) ) ;
#391 = CARTESIAN_POINT ( 'NONE',  ( 22.49448184590488609, 22.22300645049885048, 5.637851296924623057E-15 ) ) ;
#392 = EDGE_LOOP ( 'NONE', ( #9098, #8342, #7823, #504 ) ) ;
#393 = ORIENTED_EDGE ( 'NONE', *, *, #4024, .T. ) ;
#394 = AXIS2_PLACEMENT_3D ( 'NONE', #10889, #13103, #12895 ) ;
#395 = ORIENTED_EDGE ( 'NONE', *, *, #12190, .T. ) ;
#396 = DIRECTION ( 'NONE',  ( -0.000000000000000000, -1.000000000000000000, -0.000000000000000000 ) ) ;
#397 = VERTEX_POINT ( 'NONE', #7385 ) ;
#398 = CARTESIAN_POINT ( 'NONE',  ( 15.29705854078139815, 0.8232575913728894523, 1.873561326908940224E-15 ) ) ;
#399 = CARTESIAN_POINT ( 'NONE',  ( -13.79311422413708499, -21.62638421600851046, -7.500000000000000000 ) ) ;
#400 = EDGE_CURVE ( 'NONE', #6752, #9552, #11414, .T. ) ;
#401 = DIRECTION ( 'NONE',  ( 1.000000000000000000, 0.000000000000000000, 0.000000000000000000 ) ) ;
#402 = CARTESIAN_POINT ( 'NONE',  ( 1.947606478028208261E-13, -70.00000000000000000, 2.411204079342396664E-14 ) ) ;
#403 = DIRECTION ( 'NONE',  ( 0.000000000000000000, 0.000000000000000000, 1.000000000000000000 ) ) ;
#404 = CARTESIAN_POINT ( 'NONE',  ( 34.99999999999958789, 1.104930248025249758E-13, -2.499999999999999112 ) ) ;
#405 = DIRECTION ( 'NONE',  ( -1.000000000000000000, 0.000000000000000000, 0.000000000000000000 ) ) ;
#406 = EDGE_CURVE ( 'NONE', #397, #11234, #4095, .T. ) ;
#407 = B_SPLINE_CURVE_WITH_KNOTS ( 'NONE', 3,
 ( #6684, #183, #7665, #5554 ),
 .UNSPECIFIED., .F., .F.,
 ( 4, 4 ),
 ( 0.000000000000000000, 1.000000000000000000 ),
 .UNSPECIFIED. ) ;
#408 = FACE_OUTER_BOUND ( 'NONE', #9520, .T. ) ;
#409 = LINE ( 'NONE', #6624, #13262 ) ;
#410 = DIRECTION ( 'NONE',  ( 0.000000000000000000, 0.000000000000000000, 1.000000000000000000 ) ) ;
#411 = FILL_AREA_STYLE_COLOUR ( '', #8311 ) ;
#412 = DIRECTION ( 'NONE',  ( 0.9960067511297463483, -0.08927794634716620936, 4.818676322152979407E-17 ) ) ;
#413 = CYLINDRICAL_SURFACE ( 'NONE', #5659, 8.385254915620292238 ) ;
#414 = CARTESIAN_POINT ( 'NONE',  ( 39.06230589874904524, 109.5835921350012683, 2.499999999999999556 ) ) ;
#415 = EDGE_LOOP ( 'NONE', ( #5034, #4687, #8692, #5104 ) ) ;
#416 = CARTESIAN_POINT ( 'NONE',  ( -25.00000000000000355, 120.0000000000000284, -2.500000000000000000 ) ) ;
#417 = EDGE_LOOP ( 'NONE', ( #8624, #1326, #7821, #12079 ) ) ;
#418 = ORIENTED_EDGE ( 'NONE', *, *, #4130, .F. ) ;
#419 = PLANE ( 'NONE',  #6579 ) ;
#420 = VERTEX_POINT ( 'NONE', #8511 ) ;
#421 = LINE ( 'NONE', #1380, #11465 ) ;
#422 = CARTESIAN_POINT ( 'NONE',  ( -39.31777158827905794, 101.3359913474317011, 2.434761661425243418 ) ) ;
#423 = CARTESIAN_POINT ( 'NONE',  ( -8.385254915620299343, -34.41905512736551032, 16.77050983124059513 ) ) ;
#424 = CARTESIAN_POINT ( 'NONE',  ( -11.81226048336476708, -40.00941361824963849, -1.520867253700650540E-15 ) ) ;
#425 = VERTEX_POINT ( 'NONE', #1859 ) ;
#426 = FILL_AREA_STYLE ('',( #13278 ) ) ;
#427 = EDGE_LOOP ( 'NONE', ( #12636, #418, #9896, #533 ) ) ;
#428 = CIRCLE ( 'NONE', #8039, 2.000000000000003997 ) ;
#429 = DIRECTION ( 'NONE',  ( 0.000000000000000000, 0.000000000000000000, 1.000000000000000000 ) ) ;
#430 = VERTEX_POINT ( 'NONE', #6149 ) ;
#431 = ORIENTED_EDGE ( 'NONE', *, *, #8075, .F. ) ;
#432 = ADVANCED_FACE ( 'NONE', ( #819 ), #1931, .T. ) ;
#433 = DIRECTION ( 'NONE',  ( -1.000000000000000000, -1.224646799147353207E-16, 0.000000000000000000 ) ) ;
#434 = DIRECTION ( 'NONE',  ( 0.9960067511297463483, -0.08927794634716620936, 4.626175998653454121E-17 ) ) ;
#435 = VECTOR ( 'NONE', #12367, 1000.000000000000000 ) ;
#436 = CARTESIAN_POINT ( 'NONE',  ( -34.25812584745457201, 108.1980041606221192, -0.5000000000000000000 ) ) ;
#437 = CARTESIAN_POINT ( 'NONE',  ( 2.498436201158980463, -101.8697035856479260, 6.998341292597221930 ) ) ;
#438 = CARTESIAN_POINT ( 'NONE',  ( 15.29705854078138927, 17.78624592198638155, -30.59411708156276788 ) ) ;
#439 = ORIENTED_EDGE ( 'NONE', *, *, #8493, .T. ) ;
#440 = ORIENTED_EDGE ( 'NONE', *, *, #1952, .T. ) ;
#441 = ORIENTED_EDGE ( 'NONE', *, *, #13836, .T. ) ;
#442 = AXIS2_PLACEMENT_3D ( 'NONE', #5645, #10070, #6772 ) ;
#443 = CARTESIAN_POINT ( 'NONE',  ( 12.99553232110414669, -26.62435705548577047, 3.182987412051232956E-15 ) ) ;
#444 = CARTESIAN_POINT ( 'NONE',  ( 2.563982627555995819, -78.09090909091013089, 9.749794964675599473 ) ) ;
#445 = EDGE_LOOP ( 'NONE', ( #13282, #343, #13733, #11306 ) ) ;
#446 = CARTESIAN_POINT ( 'NONE',  ( -0.9875499244693202172, -80.00464164737402939, 10.06307371418729701 ) ) ;
#447 = PLANE ( 'NONE',  #3696 ) ;
#448 = EDGE_CURVE ( 'NONE', #4575, #2194, #5143, .T. ) ;
#449 = DIRECTION ( 'NONE',  ( -2.797435172181481150E-17, 1.000000000000000000, -1.765856845898762549E-18 ) ) ;
#450 = DIRECTION ( 'NONE',  ( -0.000000000000000000, 0.000000000000000000, -1.000000000000000000 ) ) ;
#451 = CARTESIAN_POINT ( 'NONE',  ( -2.054569550994074234, -122.9090909090864159, -4.917417506340981959 ) ) ;
#452 = EDGE_CURVE ( 'NONE', #1107, #10314, #12672, .T. ) ;
#453 = DIRECTION ( 'NONE',  ( -0.5999999999999999778, -0.8000000000000000444, 2.220446049250313081E-15 ) ) ;
#454 = AXIS2_PLACEMENT_3D ( 'NONE', #3228, #2248, #4282 ) ;
#455 = DIRECTION ( 'NONE',  ( -0.8907235428302473501, -0.4545454545454531425, -0.000000000000000000 ) ) ;
#456 = EDGE_CURVE ( 'NONE', #10530, #1244, #10744, .T. ) ;
#457 = FACE_OUTER_BOUND ( 'NONE', #1, .T. ) ;
#458 = EDGE_CURVE ( 'NONE', #11452, #4720, #10511, .T. ) ;
#459 = ORIENTED_EDGE ( 'NONE', *, *, #3702, .T. ) ;
#460 = ORIENTED_EDGE ( 'NONE', *, *, #2158, .F. ) ;
#461 = AXIS2_PLACEMENT_3D ( 'NONE', #7793, #1638, #3808 ) ;
#462 = CARTESIAN_POINT ( 'NONE',  ( -4.974937185533102380, 90.00000000000000000, 0.5000000000000000000 ) ) ;
#463 = ORIENTED_EDGE ( 'NONE', *, *, #1893, .F. ) ;
#464 = CARTESIAN_POINT ( 'NONE',  ( -2.127113563276592512, -126.4347724850053396, 3.943208343314429154 ) ) ;
#465 = CARTESIAN_POINT ( 'NONE',  ( 24.37649275748779232, -100.0000000000000000, -7.500000000000000000 ) ) ;
#466 = AXIS2_PLACEMENT_3D ( 'NONE', #1579, #9018, #13326 ) ;
#467 = DIRECTION ( 'NONE',  ( 1.000000000000000000, 0.000000000000000000, 0.000000000000000000 ) ) ;
#468 = ORIENTED_EDGE ( 'NONE', *, *, #11757, .F. ) ;
#469 = DIRECTION ( 'NONE',  ( -6.158143864569485777E-17, -2.736152283717910599E-16, 1.000000000000000000 ) ) ;
#470 = VERTEX_POINT ( 'NONE', #11938 ) ;
#471 = CARTESIAN_POINT ( 'NONE',  ( -1.823748309627396313, -150.1894710958037251, 0.6860160126068575170 ) ) ;
#472 = VECTOR ( 'NONE', #11869, 1000.000000000000000 ) ;
#473 = VECTOR ( 'NONE', #3861, 1000.000000000000000 ) ;
#474 = CARTESIAN_POINT ( 'NONE',  ( 15.29705854078139282, 46.06057977201469100, -30.59411708156277854 ) ) ;
#475 = CARTESIAN_POINT ( 'NONE',  ( -2.517691654963332357E-15, 90.00000000000000000, -1.589271161308885878E-16 ) ) ;
#476 = CARTESIAN_POINT ( 'NONE',  ( -15.29705854078139105, 8.361467971976981772, -1.476515546007874940E-17 ) ) ;
#477 = CARTESIAN_POINT ( 'NONE',  ( 34.00000000000001421, 108.0000000000000142, 0.5000000000000000000 ) ) ;
#478 = DIRECTION ( 'NONE',  ( 0.8000000000000000444, 0.5999999999999999778, 0.000000000000000000 ) ) ;
#479 = DIRECTION ( 'NONE',  ( 0.7999999999999997113, 0.6000000000000003109, 0.000000000000000000 ) ) ;
#480 = EDGE_CURVE ( 'NONE', #8890, #9552, #12010, .T. ) ;
#481 = CARTESIAN_POINT ( 'NONE',  ( -10.69346802281034670, -35.22415542633469698, -1.185170506590736236E-15 ) ) ;
#482 = CIRCLE ( 'NONE', #702, 8.385254915620295790 ) ;
#483 = CARTESIAN_POINT ( 'NONE',  ( 8.385254915620288685, 15.32944684068712782, 16.77050983124058448 ) ) ;
#484 = AXIS2_PLACEMENT_3D ( 'NONE', #235, #2386, #11795 ) ;
#485 = ORIENTED_EDGE ( 'NONE', *, *, #4050, .T. ) ;
#486 = CARTESIAN_POINT ( 'NONE',  ( 4.268720428656451737, 91.34229515271626099, 2.603909174561179540 ) ) ;
#487 = ORIENTED_EDGE ( 'NONE', *, *, #12528, .F. ) ;
#488 = CARTESIAN_POINT ( 'NONE',  ( -4.607646589138113313, -134.6363636363689977, -0.3820433400546732750 ) ) ;
#489 = EDGE_LOOP ( 'NONE', ( #11904, #251, #1201, #2372 ) ) ;
#490 = DIRECTION ( 'NONE',  ( -6.158143864569485777E-17, -2.736152283717910599E-16, 1.000000000000000000 ) ) ;
#491 = AXIS2_PLACEMENT_3D ( 'NONE', #12908, #6506, #11038 ) ;
#492 = PRODUCT_CONTEXT ( 'NONE', #10764, 'mechanical' ) ;
#493 = EDGE_LOOP ( 'NONE', ( #6586, #7920, #2712, #2336 ) ) ;
#494 =( BOUNDED_SURFACE ( )  B_SPLINE_SURFACE ( 3, 3, ( 
 ( #12028, #7814, #12101, #1510 ),
 ( #10005, #4668, #11125, #3609 ),
 ( #6845, #5793, #8499, #5617 ),
 ( #306, #10669, #3167, #13002 ) ),
 .UNSPECIFIED., .F., .F., .T. ) 
 B_SPLINE_SURFACE_WITH_KNOTS ( ( 4, 4 ),
 ( 4, 4 ),
 ( 0.000000000000000000, 1.000000000000000000 ),
 ( 0.000000000000000000, 1.000000000000000000 ),
 .UNSPECIFIED. ) 
 GEOMETRIC_REPRESENTATION_ITEM ( )  RATIONAL_B_SPLINE_SURFACE ( (
 ( 1.000000000000000000, 0.3333333333333334259, 0.3333333333333334259, 1.000000000000000000),
 ( 1.000000000000000000, 0.3333333333333334259, 0.3333333333333334259, 1.000000000000000000),
 ( 1.000000000000000000, 0.3333333333333334259, 0.3333333333333334259, 1.000000000000000000),
 ( 1.000000000000000000, 0.3333333333333334259, 0.3333333333333334259, 1.000000000000000000) ) ) 
 REPRESENTATION_ITEM ( '' )  SURFACE ( )  );
#495 = CARTESIAN_POINT ( 'NONE',  ( 6.356408395747725315, -164.3636363623434704, 0.5463072363203682613 ) ) ;
#496 = AXIS2_PLACEMENT_3D ( 'NONE', #1680, #5966, #3555 ) ;
#497 = AXIS2_PLACEMENT_3D ( 'NONE', #8411, #12702, #2812 ) ;
#498 = CARTESIAN_POINT ( 'NONE',  ( -15.29705854078139105, 8.361467971976955127, -1.902879688753918396E-15 ) ) ;
#499 = CARTESIAN_POINT ( 'NONE',  ( -40.33442208022856335, 100.7954446087838107, 1.738653613625529948 ) ) ;
#500 = ADVANCED_FACE ( 'NONE', ( #7521 ), #3866, .T. ) ;
#501 = CARTESIAN_POINT ( 'NONE',  ( 15.29705854078138927, 19.67281349139177138, 3.746698755667522411E-15 ) ) ;
#502 = CARTESIAN_POINT ( 'NONE',  ( 9.943536536256114999, -71.42980831100965133, 1.832023074086042591 ) ) ;
#503 = ADVANCED_FACE ( 'NONE', ( #5628, #46 ), #2266, .T. ) ;
#504 = ORIENTED_EDGE ( 'NONE', *, *, #7116, .F. ) ;
#505 = CIRCLE ( 'NONE', #4061, 14.99999999999999112 ) ;
#506 = DIRECTION ( 'NONE',  ( -0.000000000000000000, -0.000000000000000000, -1.000000000000000000 ) ) ;
#507 = ORIENTED_EDGE ( 'NONE', *, *, #12353, .T. ) ;
#508 = CARTESIAN_POINT ( 'NONE',  ( 17.38503225228318883, -6.421675190136375555, 2.499999999999996891 ) ) ;
#509 = DIRECTION ( 'NONE',  ( -1.224646799147353207E-16, 1.000000000000000000, -0.000000000000000000 ) ) ;
#510 = CARTESIAN_POINT ( 'NONE',  ( -35.00000000000000000, -20.00000000000000000, 7.500000000000000000 ) ) ;
#511 = AXIS2_PLACEMENT_3D ( 'NONE', #4639, #8923, #13227 ) ;
#512 = CARTESIAN_POINT ( 'NONE',  ( -34.28542361028948449, 108.1059200568371494, -1.103255912984088427 ) ) ;
#513 = CARTESIAN_POINT ( 'NONE',  ( 6.374040420648922733, -86.95534703849641289, -6.729367440589365756 ) ) ;
#514 = CARTESIAN_POINT ( 'NONE',  ( -12.99553232110414136, 58.19864449459907974, -1.797034655631248355E-15 ) ) ;
#515 = ORIENTED_EDGE ( 'NONE', *, *, #7707, .T. ) ;
#516 = ORIENTED_EDGE ( 'NONE', *, *, #10493, .T. ) ;
#517 = EDGE_CURVE ( 'NONE', #3335, #6792, #6412, .T. ) ;
#518 = CARTESIAN_POINT ( 'NONE',  ( 6.257768754720297677E-16, -22.36966495935058319, 3.950162600893091522E-17 ) ) ;
#519 = B_SPLINE_SURFACE_WITH_KNOTS ( 'NONE', 3, 3, ( 
 ( #5541, #1213, #3438, #3236 ),
 ( #3372, #6601, #1154, #100 ),
 ( #236, #4497, #2388, #13153 ),
 ( #4353, #8636, #3301, #6541 ),
 ( #1337, #5620, #7580, #11861 ),
 ( #10799, #5478, #13452, #3655 ),
 ( #6953, #655, #9134, #5764 ),
 ( #7867, #2753, #3733, #4922 ),
 ( #12226, #3577, #13527, #5692 ),
 ( #3799, #7024, #12429, #3867 ),
 ( #10045, #12368, #1699, #12149 ),
 ( #11301, #9205, #451, #11167 ),
 ( #4790, #10184, #8150, #4713 ),
 ( #8016, #5841, #5987, #2820 ),
 ( #8086, #12293, #10119, #8924 ),
 ( #9066, #1553, #10252, #11015 ),
 ( #1415, #11241, #9978, #388 ),
 ( #1627, #528, #2683, #4640 ),
 ( #13228, #2541, #6817, #11092 ),
 ( #1486, #8999, #13303, #7941 ),
 ( #2615, #6888, #13384, #5911 ),
 ( #594, #4858, #11641, #5193 ),
 ( #8216, #4199, #2962, #1762 ),
 ( #2039, #12712, #6317, #1970 ) ),
 .UNSPECIFIED., .F., .F., .F.,
 ( 4, 1, 1, 1, 1, 1, 1, 1, 1, 1, 1, 1, 1, 1, 1, 1, 1, 1, 1, 1, 1, 4 ),
 ( 4, 4 ),
 ( -0.1668267180224854429, -0.1624291228870498593, -0.1587644602741868916, -0.1580315277516142758, -0.1536339326161787200, -0.1471422445591071271, -0.1404411472098719693, -0.1360435520744364135, -0.1316459569390008300, -0.1272483618035652464, -0.1228507666681296628, -0.1140555763972585096, -0.1096579812618229399, -0.1052603861263873564, -0.1008627909909517867, -0.09646519585551620313, -0.08976409850628105924, -0.08327241044920946633, -0.07887481531377389665, -0.07814188279120132252, -0.07447722017833831309, -0.07007962504290274341 ),
 ( 0.003200000000000001888, 0.006800000000000002223 ),
 .UNSPECIFIED. ) ;
#520 = ORIENTED_EDGE ( 'NONE', *, *, #4473, .T. ) ;
#521 = DIRECTION ( 'NONE',  ( 0.000000000000000000, 0.000000000000000000, 1.000000000000000000 ) ) ;
#522 = CARTESIAN_POINT ( 'NONE',  ( -0.2899689842973289244, -81.00000000000004263, 10.01379011345948378 ) ) ;
#523 = ORIENTED_EDGE ( 'NONE', *, *, #13758, .T. ) ;
#524 = CARTESIAN_POINT ( 'NONE',  ( -22.00000000000000000, -35.00000000000000000, 7.500000000000000000 ) ) ;
#525 = LINE ( 'NONE', #10042, #3224 ) ;
#526 = CARTESIAN_POINT ( 'NONE',  ( 34.99999999999958789, 1.104930248025249758E-13, -2.499999999999999112 ) ) ;
#527 = CARTESIAN_POINT ( 'NONE',  ( -4.918402716924988205, -70.00000000000000000, 0.8996192050778424321 ) ) ;
#528 = CARTESIAN_POINT ( 'NONE',  ( 9.844122869699651446, -91.60173160172368512, 1.011447867174433579 ) ) ;
#529 = DIRECTION ( 'NONE',  ( -2.797435172181481150E-17, 1.000000000000000000, -1.765856845898762549E-18 ) ) ;
#530 = CARTESIAN_POINT ( 'NONE',  ( 19.06870874253413461, 13.90050210118286245, -2.499999999999996447 ) ) ;
#531 = FACE_OUTER_BOUND ( 'NONE', #4485, .T. ) ;
#532 = ORIENTED_EDGE ( 'NONE', *, *, #6100, .T. ) ;
#533 = ORIENTED_EDGE ( 'NONE', *, *, #2253, .T. ) ;
#534 = VERTEX_POINT ( 'NONE', #109 ) ;
#535 = CARTESIAN_POINT ( 'NONE',  ( 18.54049621773915746, -20.00000000000000000, -7.500000000000000000 ) ) ;
#536 = ORIENTED_EDGE ( 'NONE', *, *, #1893, .T. ) ;
#537 = ADVANCED_FACE ( 'NONE', ( #13013 ), #3342, .F. ) ;
#538 = CARTESIAN_POINT ( 'NONE',  ( 6.100791518294768956, -112.6832912522008030, 0.2938029233185053268 ) ) ;
#539 = FACE_OUTER_BOUND ( 'NONE', #7622, .T. ) ;
#540 = EDGE_CURVE ( 'NONE', #2953, #6457, #12760, .T. ) ;
#541 = CARTESIAN_POINT ( 'NONE',  ( -10.69346802281034847, 30.74929022373126841, -1.418169827888134119E-15 ) ) ;
#542 = DIRECTION ( 'NONE',  ( -1.000000000000000000, 0.000000000000000000, 0.000000000000000000 ) ) ;
#543 = EDGE_CURVE ( 'NONE', #5663, #11307, #11801, .T. ) ;
#544 = CARTESIAN_POINT ( 'NONE',  ( 52.82363224725100537, -5.817485239812894449, 2.500000000000000000 ) ) ;
#545 = ORIENTED_EDGE ( 'NONE', *, *, #289, .F. ) ;
#546 = CARTESIAN_POINT ( 'NONE',  ( -0.1618148777053960430, -158.9590251630839646, -1.491571185530413901 ) ) ;
#547 = CARTESIAN_POINT ( 'NONE',  ( 4.804060984082277663, 90.20500167315060480, -1.391503737930617213 ) ) ;
#548 = CARTESIAN_POINT ( 'NONE',  ( 35.00000000000000711, -25.00000000000000000, 7.500000000000000000 ) ) ;
#549 = CARTESIAN_POINT ( 'NONE',  ( 8.385254915620294014, 22.12961257269105531, -16.77050983124058092 ) ) ;
#550 = CYLINDRICAL_SURFACE ( 'NONE', #13175, 4.999999999999997335 ) ;
#551 = CIRCLE ( 'NONE', #1870, 4.999999999999997335 ) ;
#552 = CARTESIAN_POINT ( 'NONE',  ( -19.36040733361899768, 26.87219970003945591, -5.058700639371027208 ) ) ;
#553 = CARTESIAN_POINT ( 'NONE',  ( -12.99579180576517601, 64.08350967699263379, 25.99158361153033070 ) ) ;
#554 = DIRECTION ( 'NONE',  ( -2.797435172181481150E-17, 1.000000000000000000, -1.765856845898762549E-18 ) ) ;
#555 = CARTESIAN_POINT ( 'NONE',  ( -13.62402331790689836, -89.44155844156966850, 2.236035847434436619 ) ) ;
#556 = EDGE_CURVE ( 'NONE', #5704, #4432, #4456, .T. ) ;
#557 = ORIENTED_EDGE ( 'NONE', *, *, #6920, .T. ) ;
#558 = AXIS2_PLACEMENT_3D ( 'NONE', #878, #13613, #12600 ) ;
#559 = CARTESIAN_POINT ( 'NONE',  ( -9.701113296676140862, -68.99999999999997158, -3.021359762293432283 ) ) ;
#560 = EDGE_CURVE ( 'NONE', #8899, #4393, #6700, .T. ) ;
#561 = DIRECTION ( 'NONE',  ( -1.000000000000000000, 0.000000000000000000, 0.000000000000000000 ) ) ;
#562 = B_SPLINE_CURVE_WITH_KNOTS ( 'NONE', 3,
 ( #7847, #8980, #2601, #8064, #5745, #4693, #3713, #8001, #12352, #6877, #8206, #9051, #6036, #1537, #2741, #513, #4846, #3785, #7009, #3636, #1686, #13571, #3924, #11152, #11223, #11290, #2873, #5822, #12276, #12488, #5899, #7927, #7147, #11425, #10101, #1614, #5971, #10026, #4774, #2664, #437, #10172, #13509, #13287, #3851, #12210, #13365, #10239, #643, #9121, #6933, #583, #13437, #4907, #9185, #8134, #12418, #2807, #7079, #10311, #11357, #1749, #712, #4976, #9255, #4123, #10374, #4184, #8340, #2088, #8538, #1820, #10575, #9592, #10504, #12564, #7418, #8405, #1932, #9327, #3007, #13642, #2947, #5244, #7214, #5046, #1886, #11496, #6369, #977, #11564, #4255, #6237, #1051, #6175, #11695, #12840, #10443, #1955, #3988, #9466, #13713, #8270, #12634, #9531, #13841, #843, #4059 ),
 .UNSPECIFIED., .F., .F.,
 ( 4, 2, 2, 2, 2, 2, 2, 2, 2, 2, 2, 2, 2, 2, 2, 2, 2, 2, 2, 2, 2, 2, 2, 2, 2, 2, 2, 2, 2, 2, 2, 2, 2, 2, 2, 2, 2, 2, 2, 2, 2, 2, 2, 2, 2, 2, 2, 2, 2, 2, 2, 2, 2, 4 ),
 ( 8.420559318810145779E-18, 0.0007945603842730117761, 0.001589120768546015095, 0.003178241537091996798, 0.004767362305637979150, 0.006356483074183960635, 0.009534724611275923606, 0.01112384537982191897, 0.01271296614836791260, 0.01430208691691390623, 0.01589120768545989465, 0.01906944922255190966, 0.02065856999109790329, 0.02224769075964389692, 0.02383681152818988708, 0.02542593229673587724, 0.02860417383382784021, 0.03019329460237380608, 0.03178241537091977542, 0.03337153613946574476, 0.03496065690801170717, 0.03813889844510363891, 0.03972801921364962213, 0.04131713998219560535, 0.04449538151928759955, 0.04767362305637958680, 0.04926274382492558390, 0.05085186459347158100, 0.05403010613056356826, 0.05561922689910957923, 0.05720834766765561102, 0.05879746843620162200, 0.06038658920474763991, 0.06356483074183967574, 0.06515395151038569366, 0.06674307227893173933, 0.06992131381602378903, 0.07309955535311585262, 0.07468867612166184278, 0.07627779689020783294, 0.07945603842729982713, 0.08104515919584577566, 0.08263427996439172418, 0.08581252150148363511, 0.08899076303857555992, 0.09057988380712146681, 0.09216900457566738758, 0.09375812534421329447, 0.09534724611275921524, 0.09693636688130513601, 0.09852548764985105678, 0.1001146084183969637, 0.1009091688026699241, 0.1017037291869428844 ),
 .UNSPECIFIED. ) ;
#563 = CARTESIAN_POINT ( 'NONE',  ( 13.62402331790597287, -89.44155844157094748, -2.236035847433821555 ) ) ;
#564 = CARTESIAN_POINT ( 'NONE',  ( 10.69381717166375090, 6.709890972096426154, 21.38763434332751245 ) ) ;
#565 = CARTESIAN_POINT ( 'NONE',  ( -12.99579180576517246, -20.73949187309215247, -1.518279536322449159E-15 ) ) ;
#566 = DIRECTION ( 'NONE',  ( 0.9960067511297464593, -0.08927794634716622324, 3.401418580343279473E-17 ) ) ;
#567 = CARTESIAN_POINT ( 'NONE',  ( -35.00000000000000000, -4.286263797015736496E-15, -7.500000000000000000 ) ) ;
#568 = AXIS2_PLACEMENT_3D ( 'NONE', #1899, #1829, #13782 ) ;
#569 = ORIENTED_EDGE ( 'NONE', *, *, #2135, .F. ) ;
#570 = ORIENTED_EDGE ( 'NONE', *, *, #12778, .T. ) ;
#571 = EDGE_CURVE ( 'NONE', #1705, #2048, #9846, .T. ) ;
#572 = CARTESIAN_POINT ( 'NONE',  ( 10.69346802281034670, 30.74929022373126841, 0.000000000000000000 ) ) ;
#573 = EDGE_CURVE ( 'NONE', #11806, #2481, #9618, .T. ) ;
#574 = CIRCLE ( 'NONE', #8391, 22.49999999999999289 ) ;
#575 = VERTEX_POINT ( 'NONE', #2474 ) ;
#576 = VERTEX_POINT ( 'NONE', #10197 ) ;
#577 = SURFACE_STYLE_FILL_AREA ( #12131 ) ;
#578 = TOROIDAL_SURFACE ( 'NONE', #8393, 17.49999999999999645, 5.000000000000000000 ) ;
#579 = CARTESIAN_POINT ( 'NONE',  ( -41.00000000000000000, -4.286263797015736496E-15, 7.500000000000000000 ) ) ;
#580 = AXIS2_PLACEMENT_3D ( 'NONE', #9356, #5931, #7955 ) ;
#581 = CARTESIAN_POINT ( 'NONE',  ( 19.75162188639114902, 26.77857048203552992, -3.206191164072788702 ) ) ;
#582 = DIRECTION ( 'NONE',  ( -1.000000000000000000, -0.000000000000000000, -0.000000000000000000 ) ) ;
#583 = CARTESIAN_POINT ( 'NONE',  ( -5.285683233297803874, -111.9165838417090271, 3.246843445714708398 ) ) ;
#584 = CARTESIAN_POINT ( 'NONE',  ( 10.69346802281034670, 49.59884612375012125, 1.251549203118916541E-15 ) ) ;
#585 = AXIS2_PLACEMENT_3D ( 'NONE', #8584, #7391, #10614 ) ;
#586 = VECTOR ( 'NONE', #4081, 1000.000000000000000 ) ;
#587 = DIRECTION ( 'NONE',  ( -0.000000000000000000, -0.000000000000000000, -1.000000000000000000 ) ) ;
#588 = CARTESIAN_POINT ( 'NONE',  ( 0.9402774206043281735, -80.12121212121192571, 9.996606859377758170 ) ) ;
#589 = ORIENTED_EDGE ( 'NONE', *, *, #13115, .F. ) ;
#590 = CARTESIAN_POINT ( 'NONE',  ( 0.2039588443089787317, -79.18543989864099331, 10.12004280280962831 ) ) ;
#591 = SURFACE_STYLE_USAGE ( .BOTH. , #5908 ) ;
#592 = CARTESIAN_POINT ( 'NONE',  ( 34.06230589874905235, 109.5835921350012683, 7.500000000000000000 ) ) ;
#593 = CARTESIAN_POINT ( 'NONE',  ( -42.16244658108818300, 105.4500712252157797, -2.499999999999999556 ) ) ;
#594 = CARTESIAN_POINT ( 'NONE',  ( -7.328281204033265439, -76.12121212249812174, -4.753922619039316011 ) ) ;
#595 = DIRECTION ( 'NONE',  ( -1.224646799147353207E-16, 1.000000000000000000, -0.000000000000000000 ) ) ;
#596 = DIRECTION ( 'NONE',  ( 0.000000000000000000, 1.000000000000000000, 2.775557561562888984E-15 ) ) ;
#597 = CARTESIAN_POINT ( 'NONE',  ( 1.224646799147353217E-14, -100.0000000000000000, 0.000000000000000000 ) ) ;
#598 = AXIS2_PLACEMENT_3D ( 'NONE', #9274, #3873, #2045 ) ;
#599 = EDGE_LOOP ( 'NONE', ( #7641, #485, #11774, #148, #4430, #5510 ) ) ;
#600 = ORIENTED_EDGE ( 'NONE', *, *, #540, .F. ) ;
#601 = ORIENTED_EDGE ( 'NONE', *, *, #5658, .F. ) ;
#602 = ORIENTED_EDGE ( 'NONE', *, *, #12372, .T. ) ;
#603 = CARTESIAN_POINT ( 'NONE',  ( -1.619020611652117081, -125.5321122364420603, 4.300443607797105550 ) ) ;
#604 = VECTOR ( 'NONE', #12351, 1000.000000000000000 ) ;
#605 = DIRECTION ( 'NONE',  ( 0.000000000000000000, 0.000000000000000000, 1.000000000000000000 ) ) ;
#606 = CARTESIAN_POINT ( 'NONE',  ( -1.604942417060130136E-15, 57.37192529142945574, -1.013106070382630377E-16 ) ) ;
#607 = ORIENTED_EDGE ( 'NONE', *, *, #7807, .T. ) ;
#608 = ORIENTED_EDGE ( 'NONE', *, *, #9776, .F. ) ;
#609 = CARTESIAN_POINT ( 'NONE',  ( 34.99999999999958789, 1.104930248025249758E-13, -2.499999999999999112 ) ) ;
#610 = FACE_OUTER_BOUND ( 'NONE', #6249, .T. ) ;
#611 = CARTESIAN_POINT ( 'NONE',  ( 4.942648287111185645, 90.01344868170882307, -0.7664870281642336414 ) ) ;
#612 = DIRECTION ( 'NONE',  ( -2.797435172181481150E-17, 1.000000000000000000, -1.765856845898762549E-18 ) ) ;
#613 = FACE_OUTER_BOUND ( 'NONE', #10515, .T. ) ;
#614 = EDGE_CURVE ( 'NONE', #8676, #13485, #6969, .T. ) ;
#615 = DIRECTION ( 'NONE',  ( -0.000000000000000000, -0.000000000000000000, -1.000000000000000000 ) ) ;
#616 = LINE ( 'NONE', #8236, #7848 ) ;
#617 = DIRECTION ( 'NONE',  ( 0.000000000000000000, 0.000000000000000000, -1.000000000000000000 ) ) ;
#618 = VERTEX_POINT ( 'NONE', #399 ) ;
#619 = CARTESIAN_POINT ( 'NONE',  ( 4.231485814931493117, 91.18833760977217651, 2.665113332093635101 ) ) ;
#620 = ORIENTED_EDGE ( 'NONE', *, *, #5753, .T. ) ;
#621 = CARTESIAN_POINT ( 'NONE',  ( -3.373786045844842096, -82.89610389617892849, 3.887588323745183150 ) ) ;
#622 = ORIENTED_EDGE ( 'NONE', *, *, #7115, .F. ) ;
#623 = CIRCLE ( 'NONE', #12020, 24.99999999999998934 ) ;
#624 = VERTEX_POINT ( 'NONE', #6894 ) ;
#625 = CARTESIAN_POINT ( 'NONE',  ( 42.49999999999999289, 120.0000000000000142, -7.500000000000000000 ) ) ;
#626 = FACE_OUTER_BOUND ( 'NONE', #13070, .T. ) ;
#627 = CARTESIAN_POINT ( 'NONE',  ( -5.581994045268341864, -105.1818181818167091, 11.80851735648757739 ) ) ;
#628 = EDGE_CURVE ( 'NONE', #12494, #2284, #10129, .T. ) ;
#629 = DIRECTION ( 'NONE',  ( 0.4545454545454531425, -0.8907235428302472391, 0.000000000000000000 ) ) ;
#630 = CARTESIAN_POINT ( 'NONE',  ( 0.000000000000000000, 71.01020514433645303, -0.5000000000000000000 ) ) ;
#631 = ADVANCED_FACE ( 'NONE', ( #539 ), #4652, .T. ) ;
#632 = EDGE_CURVE ( 'NONE', #3638, #2716, #12550, .T. ) ;
#633 = CARTESIAN_POINT ( 'NONE',  ( 8.385254915620294014, 90.00000000000000000, 8.679704431140118580E-16 ) ) ;
#634 = CYLINDRICAL_SURFACE ( 'NONE', #4434, 15.29705854078138749 ) ;
#635 = ADVANCED_FACE ( 'NONE', ( #5923, #12382 ), #2768, .F. ) ;
#636 = EDGE_CURVE ( 'NONE', #4358, #10177, #6755, .T. ) ;
#637 = ORIENTED_EDGE ( 'NONE', *, *, #9772, .T. ) ;
#638 = ORIENTED_EDGE ( 'NONE', *, *, #13760, .T. ) ;
#639 = SURFACE_SIDE_STYLE ('',( #577 ) ) ;
#640 = CARTESIAN_POINT ( 'NONE',  ( -34.99999999999999289, -135.0000000000000000, 0.000000000000000000 ) ) ;
#641 = CARTESIAN_POINT ( 'NONE',  ( -8.862685976966703905, -71.63821982307230485, -4.927609701037551027 ) ) ;
#642 = CARTESIAN_POINT ( 'NONE',  ( -39.06230589874905235, 109.5835921350012683, -2.499999999999999556 ) ) ;
#643 = CARTESIAN_POINT ( 'NONE',  ( -3.419709198711867071, -108.3206314215273665, 5.719072246552273420 ) ) ;
#644 = CARTESIAN_POINT ( 'NONE',  ( -15.29705854078138927, 17.78624592198638155, -3.776441015662857042E-15 ) ) ;
#645 = CIRCLE ( 'NONE', #8252, 15.29705854078139993 ) ;
#646 = ADVANCED_FACE ( 'NONE', ( #3590 ), #7879, .T. ) ;
#647 = ORIENTED_EDGE ( 'NONE', *, *, #9006, .T. ) ;
#648 = DIRECTION ( 'NONE',  ( -4.163336342344333082E-15, 1.000000000000000000, 1.734723475976805615E-16 ) ) ;
#649 = DIRECTION ( 'NONE',  ( -1.000000000000000000, -0.000000000000000000, -0.000000000000000000 ) ) ;
#650 = CIRCLE ( 'NONE', #9377, 22.49999999999998934 ) ;
#651 = CARTESIAN_POINT ( 'NONE',  ( 9.991007172155546456, -71.90909090909001122, 2.111483349789144981 ) ) ;
#652 = ORIENTED_EDGE ( 'NONE', *, *, #5322, .F. ) ;
#653 = DIRECTION ( 'NONE',  ( -1.000000000000000000, 0.000000000000000000, 0.000000000000000000 ) ) ;
#654 = DIRECTION ( 'NONE',  ( 0.000000000000000000, 0.000000000000000000, 1.000000000000000000 ) ) ;
#655 = CARTESIAN_POINT ( 'NONE',  ( -1.109824446838103551, -148.3982683980276533, 1.619194360872903804 ) ) ;
#656 = CARTESIAN_POINT ( 'NONE',  ( 47.16901142695026294, 17.29003067336574517, -2.499999999999993783 ) ) ;
#657 = CARTESIAN_POINT ( 'NONE',  ( -8.385254915620292238, 22.12961257269105531, -3.907772785857374249E-17 ) ) ;
#658 = CYLINDRICAL_SURFACE ( 'NONE', #13126, 25.50000000002549783 ) ;
#659 = ORIENTED_EDGE ( 'NONE', *, *, #7380, .T. ) ;
#660 = EDGE_CURVE ( 'NONE', #1806, #12845, #2964, .T. ) ;
#661 = ORIENTED_EDGE ( 'NONE', *, *, #10607, .F. ) ;
#662 = CIRCLE ( 'NONE', #206, 4.999999999999996447 ) ;
#663 = ORIENTED_EDGE ( 'NONE', *, *, #3817, .F. ) ;
#664 = CARTESIAN_POINT ( 'NONE',  ( 1.843109844542686560, -151.2149270183035128, -0.2962055024153073535 ) ) ;
#665 = ORIENTED_EDGE ( 'NONE', *, *, #2832, .F. ) ;
#666 = CARTESIAN_POINT ( 'NONE',  ( 6.132836266241635137, -110.2447350134475101, -1.893865185603917922 ) ) ;
#667 = DIRECTION ( 'NONE',  ( -0.000000000000000000, -0.000000000000000000, -1.000000000000000000 ) ) ;
#668 = CARTESIAN_POINT ( 'NONE',  ( 25.00000000000000355, 120.0000000000000142, 2.499999999999999556 ) ) ;
#669 = SPHERICAL_SURFACE ( 'NONE', #11083, 5.000000000000000000 ) ;
#670 = CARTESIAN_POINT ( 'NONE',  ( 1.369039070337584096, -125.1255798145694200, -4.439507930958486170 ) ) ;
#671 = VECTOR ( 'NONE', #4287, 1000.000000000000000 ) ;
#672 = CARTESIAN_POINT ( 'NONE',  ( 10.00000000000000000, 98.00000000000000000, -0.5000000000000000000 ) ) ;
#673 = CARTESIAN_POINT ( 'NONE',  ( -2.517691654963332357E-15, 90.00000000000000000, -1.589271161308885878E-16 ) ) ;
#674 = DIRECTION ( 'NONE',  ( -6.158143864569485777E-17, -2.736152283717910599E-16, 1.000000000000000000 ) ) ;
#675 = AXIS2_PLACEMENT_3D ( 'NONE', #13174, #7668, #12891 ) ;
#676 = DIRECTION ( 'NONE',  ( 1.000000000000000000, 3.568574007723717789E-15, 0.000000000000000000 ) ) ;
#677 = DIRECTION ( 'NONE',  ( -0.4545454545454531425, -0.8907235428302472391, 0.000000000000000000 ) ) ;
#678 = CARTESIAN_POINT ( 'NONE',  ( 8.385254915620290461, 62.45333659073423860, 2.053795118489800004E-15 ) ) ;
#679 = ORIENTED_EDGE ( 'NONE', *, *, #10110, .F. ) ;
#680 = CARTESIAN_POINT ( 'NONE',  ( -1.651792843486753513E-16, 5.904668890677672088, -1.042679998336861873E-17 ) ) ;
#681 = AXIS2_PLACEMENT_3D ( 'NONE', #12169, #3822, #11262 ) ;
#682 = ORIENTED_EDGE ( 'NONE', *, *, #7351, .F. ) ;
#683 = CARTESIAN_POINT ( 'NONE',  ( -2.937342332082010898, -95.36363636365091168, -3.570487953801811276 ) ) ;
#684 = AXIS2_PLACEMENT_3D ( 'NONE', #416, #1511, #3396 ) ;
#685 = ORIENTED_EDGE ( 'NONE', *, *, #12001, .T. ) ;
#686 = EDGE_CURVE ( 'NONE', #4911, #5054, #12997, .T. ) ;
#687 = AXIS2_PLACEMENT_3D ( 'NONE', #7573, #11991, #11787 ) ;
#688 = ORIENTED_EDGE ( 'NONE', *, *, #2950, .T. ) ;
#689 = FACE_BOUND ( 'NONE', #195, .T. ) ;
#690 = CARTESIAN_POINT ( 'NONE',  ( 0.000000000000000000, 0.000000000000000000, 0.000000000000000000 ) ) ;
#691 = CARTESIAN_POINT ( 'NONE',  ( 1.315456961488612908, -124.8181818181797098, -4.422452657364230433 ) ) ;
#692 = AXIS2_PLACEMENT_3D ( 'NONE', #9743, #2236, #1063 ) ;
#693 = FACE_OUTER_BOUND ( 'NONE', #13636, .T. ) ;
#694 = CARTESIAN_POINT ( 'NONE',  ( 25.00000000000000355, 120.0000000000000284, -0.5000000000000000000 ) ) ;
#695 = AXIS2_PLACEMENT_3D ( 'NONE', #13824, #5226, #4237 ) ;
#696 = FACE_OUTER_BOUND ( 'NONE', #7553, .T. ) ;
#697 = VECTOR ( 'NONE', #5522, 1000.000000000000000 ) ;
#698 = UNCERTAINTY_MEASURE_WITH_UNIT (LENGTH_MEASURE( 1.000000000000000082E-05 ), #1042, 'distance_accuracy_value', 'NONE');
#699 = CARTESIAN_POINT ( 'NONE',  ( -4.471182088707197799, 90.98125128669738615, 2.240943909473569917 ) ) ;
#700 = EDGE_LOOP ( 'NONE', ( #13623, #151, #5803, #4865 ) ) ;
#701 = EDGE_CURVE ( 'NONE', #1478, #9187, #6462, .T. ) ;
#702 = AXIS2_PLACEMENT_3D ( 'NONE', #7338, #908, #8404 ) ;
#703 = CARTESIAN_POINT ( 'NONE',  ( -7.331936968928880916, -85.59420029784318729, 5.937794338404503769 ) ) ;
#704 = EDGE_CURVE ( 'NONE', #3094, #2145, #2456, .T. ) ;
#705 = AXIS2_PLACEMENT_3D ( 'NONE', #8682, #11776, #4329 ) ;
#706 = AXIS2_PLACEMENT_3D ( 'NONE', #5977, #6041, #11432 ) ;
#707 = EDGE_CURVE ( 'NONE', #2716, #6241, #8627, .T. ) ;
#708 = EDGE_CURVE ( 'NONE', #4432, #2174, #1790, .T. ) ;
#709 = CARTESIAN_POINT ( 'NONE',  ( -25.00000000000000000, -35.00000000000000000, 7.500000000000000000 ) ) ;
#710 = DIRECTION ( 'NONE',  ( -0.000000000000000000, -0.000000000000000000, -1.000000000000000000 ) ) ;
#711 = DIRECTION ( 'NONE',  ( 0.000000000000000000, 1.000000000000000000, 0.000000000000000000 ) ) ;
#712 = CARTESIAN_POINT ( 'NONE',  ( -4.569026568008291989, -119.8678717589752836, -2.546033243568991633 ) ) ;
#713 = CARTESIAN_POINT ( 'NONE',  ( -4.330127018922195425, 92.00000000000000000, 2.500000000000000000 ) ) ;
#714 = VECTOR ( 'NONE', #10865, 1000.000000000000000 ) ;
#715 = AXIS2_PLACEMENT_3D ( 'NONE', #7101, #4647, #7031 ) ;
#716 = ORIENTED_EDGE ( 'NONE', *, *, #10582, .F. ) ;
#717 = VERTEX_POINT ( 'NONE', #1204 ) ;
#718 = EDGE_CURVE ( 'NONE', #5708, #13751, #11865, .T. ) ;
#719 = EDGE_CURVE ( 'NONE', #13879, #9113, #9755, .T. ) ;
#720 = DIRECTION ( 'NONE',  ( -6.158143864569485777E-17, -2.736152283717910599E-16, 1.000000000000000000 ) ) ;
#721 = CARTESIAN_POINT ( 'NONE',  ( 0.1760972876109651863, -80.66666666666658614, 10.02690338805414072 ) ) ;
#722 = EDGE_LOOP ( 'NONE', ( #11943, #9603, #12720, #1677 ) ) ;
#723 = EDGE_CURVE ( 'NONE', #5202, #2631, #4244, .T. ) ;
#724 = LINE ( 'NONE', #2959, #8363 ) ;
#725 = EDGE_CURVE ( 'NONE', #6555, #9666, #3819, .T. ) ;
#726 = AXIS2_PLACEMENT_3D ( 'NONE', #1717, #10409, #13405 ) ;
#727 = CARTESIAN_POINT ( 'NONE',  ( 40.81228451836345528, 100.6358150620708329, 0.000000000000000000 ) ) ;
#728 = CARTESIAN_POINT ( 'NONE',  ( -14.41066181492265308, -21.94006687227777874, -6.364279405527200062 ) ) ;
#729 = DIRECTION ( 'NONE',  ( -2.797435172181481150E-17, 1.000000000000000000, -1.765856845898762549E-18 ) ) ;
#730 = CYLINDRICAL_SURFACE ( 'NONE', #10911, 9.000000000008999024 ) ;
#731 = CARTESIAN_POINT ( 'NONE',  ( 58.17953216333035726, -10.62823074130461620, -8.673617379884035472E-16 ) ) ;
#732 = EDGE_LOOP ( 'NONE', ( #6280, #5930, #13577, #2245 ) ) ;
#733 = EDGE_LOOP ( 'NONE', ( #2396, #11229, #1811, #8877, #4164, #2069 ) ) ;
#734 = ORIENTED_EDGE ( 'NONE', *, *, #9467, .T. ) ;
#735 = DIRECTION ( 'NONE',  ( -1.000000000000000000, 0.000000000000000000, 0.000000000000000000 ) ) ;
#736 = ORIENTED_EDGE ( 'NONE', *, *, #8755, .F. ) ;
#737 = VECTOR ( 'NONE', #6051, 1000.000000000000000 ) ;
#738 = CARTESIAN_POINT ( 'NONE',  ( -6.341686887230054914, -95.24900142918743029, -5.248039533272778279 ) ) ;
#739 = CARTESIAN_POINT ( 'NONE',  ( -33.99999999999999289, 108.0000000000000142, 2.500000000000000000 ) ) ;
#740 = DIRECTION ( 'NONE',  ( 6.158143864569485777E-17, 2.736152283717910599E-16, -1.000000000000000000 ) ) ;
#741 = ORIENTED_EDGE ( 'NONE', *, *, #7517, .T. ) ;
#742 = CARTESIAN_POINT ( 'NONE',  ( -35.00000000000000000, -4.286263797015736496E-15, -4.000000000000000000 ) ) ;
#743 = CARTESIAN_POINT ( 'NONE',  ( -1.570139719938473233, -148.1629368621884169, 1.428393430366113881 ) ) ;
#744 = EDGE_CURVE ( 'NONE', #12212, #7540, #11649, .T. ) ;
#745 = CARTESIAN_POINT ( 'NONE',  ( -0.6059849261898251349, -166.5454546808362863, 5.665245053931520225 ) ) ;
#746 = DIRECTION ( 'NONE',  ( -2.797435172181481150E-17, 1.000000000000000000, -1.765856845898762549E-18 ) ) ;
#747 = CARTESIAN_POINT ( 'NONE',  ( -25.00000000000000355, 120.0000000000000142, -7.500000000000000000 ) ) ;
#748 = DIRECTION ( 'NONE',  ( -1.000000000000000000, 0.000000000000000000, 0.000000000000000000 ) ) ;
#749 = FACE_OUTER_BOUND ( 'NONE', #779, .T. ) ;
#750 = VERTEX_POINT ( 'NONE', #1329 ) ;
#751 = DIRECTION ( 'NONE',  ( -0.000000000000000000, -0.000000000000000000, -1.000000000000000000 ) ) ;
#752 = VERTEX_POINT ( 'NONE', #11007 ) ;
#753 = CARTESIAN_POINT ( 'NONE',  ( 3.784192700541107346, -60.99999999999997158, 1.982393907671070599 ) ) ;
#754 = VECTOR ( 'NONE', #380, 1000.000000000000000 ) ;
#755 = ORIENTED_EDGE ( 'NONE', *, *, #6867, .F. ) ;
#756 = ORIENTED_EDGE ( 'NONE', *, *, #708, .T. ) ;
#757 = DIRECTION ( 'NONE',  ( -2.797435172181481150E-17, 1.000000000000000000, -1.765856845898762549E-18 ) ) ;
#758 = DIRECTION ( 'NONE',  ( -1.000000000000000000, 0.000000000000000000, 0.000000000000000000 ) ) ;
#759 = CIRCLE ( 'NONE', #7467, 5.000000000000004441 ) ;
#760 =( REPRESENTATION_RELATIONSHIP ('NONE','NONE', #9450, #3787 ) REPRESENTATION_RELATIONSHIP_WITH_TRANSFORMATION ( #1518 )SHAPE_REPRESENTATION_RELATIONSHIP( ) );
#761 = CARTESIAN_POINT ( 'NONE',  ( -8.385254915620286909, 34.17900274070598243, -16.77050983124057737 ) ) ;
#762 = CARTESIAN_POINT ( 'NONE',  ( -25.00000000000000355, 120.0000000000000284, -0.5000000000000000000 ) ) ;
#763 = DIRECTION ( 'NONE',  ( 1.000000000000000000, 0.000000000000000000, 0.000000000000000000 ) ) ;
#764 = CARTESIAN_POINT ( 'NONE',  ( -35.00000000000000711, -25.00000000000000711, 4.000000000000000000 ) ) ;
#765 = CARTESIAN_POINT ( 'NONE',  ( -4.974937185533102380, 90.00000000000000000, 0.5000000000000000000 ) ) ;
#766 = VECTOR ( 'NONE', #12559, 1000.000000000000000 ) ;
#767 = ORIENTED_EDGE ( 'NONE', *, *, #13181, .F. ) ;
#768 = VERTEX_POINT ( 'NONE', #9967 ) ;
#769 = VERTEX_POINT ( 'NONE', #5613 ) ;
#770 = DIRECTION ( 'NONE',  ( -2.797435172181481150E-17, 1.000000000000000000, -1.765856845898762549E-18 ) ) ;
#771 = DIRECTION ( 'NONE',  ( -6.158143864569485777E-17, -2.736152283717910599E-16, 1.000000000000000000 ) ) ;
#772 = CARTESIAN_POINT ( 'NONE',  ( 34.40223077810360763, 107.7696006147693168, 1.740676078835890372 ) ) ;
#773 = CARTESIAN_POINT ( 'NONE',  ( 10.69381717166375623, -2.714886977913000266, 1.320497585966558038E-15 ) ) ;
#774 = LINE ( 'NONE', #6035, #604 ) ;
#775 = CARTESIAN_POINT ( 'NONE',  ( 53.63671053572210923, -2.048907369402450218, -2.499999999999998224 ) ) ;
#776 = EDGE_CURVE ( 'NONE', #12557, #8762, #302, .T. ) ;
#777 = CARTESIAN_POINT ( 'NONE',  ( -35.00000000000000000, -35.00000000000000000, -7.500000000000000000 ) ) ;
#778 = EDGE_CURVE ( 'NONE', #3832, #2373, #7776, .T. ) ;
#779 = EDGE_LOOP ( 'NONE', ( #7389, #9473, #2986, #7756 ) ) ;
#780 = VERTEX_POINT ( 'NONE', #1145 ) ;
#781 = AXIS2_PLACEMENT_3D ( 'NONE', #8266, #3498, #1483 ) ;
#782 = CARTESIAN_POINT ( 'NONE',  ( -12.99579180576516890, -11.31471392308272605, -1.551565153650648068E-15 ) ) ;
#783 = ORIENTED_EDGE ( 'NONE', *, *, #6529, .T. ) ;
#784 = CARTESIAN_POINT ( 'NONE',  ( 7.500230552170977560, -73.18181818181670906, 6.960552780978377818 ) ) ;
#785 = VECTOR ( 'NONE', #10919, 1000.000000000000227 ) ;
#786 = ORIENTED_EDGE ( 'NONE', *, *, #3630, .F. ) ;
#787 = PLANE ( 'NONE',  #5436 ) ;
#788 = DIRECTION ( 'NONE',  ( -6.158143864569485777E-17, -2.736152283717910599E-16, 1.000000000000000000 ) ) ;
#789 = DIRECTION ( 'NONE',  ( -6.158143864569485777E-17, -2.736152283717910599E-16, 1.000000000000000000 ) ) ;
#790 = DIRECTION ( 'NONE',  ( 1.000000000000000000, 0.000000000000000000, 0.000000000000000000 ) ) ;
#791 = DIRECTION ( 'NONE',  ( -6.158143864569485777E-17, -2.736152283717910599E-16, 1.000000000000000000 ) ) ;
#792 = EDGE_CURVE ( 'NONE', #6662, #8229, #1784, .T. ) ;
#793 = CARTESIAN_POINT ( 'NONE',  ( 0.09329349605429697323, -158.9451967104999142, -1.495111656224116015 ) ) ;
#794 = DIRECTION ( 'NONE',  ( 0.000000000000000000, 0.000000000000000000, 1.000000000000000000 ) ) ;
#795 = CIRCLE ( 'NONE', #347, 22.99999999999999289 ) ;
#796 = EDGE_CURVE ( 'NONE', #2373, #4518, #239, .T. ) ;
#797 = ORIENTED_EDGE ( 'NONE', *, *, #9932, .F. ) ;
#798 = ORIENTED_EDGE ( 'NONE', *, *, #1974, .F. ) ;
#799 = AXIS2_PLACEMENT_3D ( 'NONE', #2482, #11030, #5781 ) ;
#800 = ORIENTED_EDGE ( 'NONE', *, *, #1340, .F. ) ;
#801 = EDGE_CURVE ( 'NONE', #3433, #1175, #9060, .T. ) ;
#802 = EDGE_CURVE ( 'NONE', #149, #11499, #5829, .T. ) ;
#803 = CARTESIAN_POINT ( 'NONE',  ( -2.332330206345282431, -138.2006080288368253, -2.072564583226628621 ) ) ;
#804 = CARTESIAN_POINT ( 'NONE',  ( 34.99999999999958789, 1.091249486606660213E-13, 2.500000000000000000 ) ) ;
#805 = VECTOR ( 'NONE', #1497, 1000.000000000000000 ) ;
#806 = CARTESIAN_POINT ( 'NONE',  ( 37.50000000000000711, 4.592425496802575156E-15, 7.500000000000000000 ) ) ;
#807 = CARTESIAN_POINT ( 'NONE',  ( 1.982309627628414228, -99.59031080125953395, 7.452550939933153984 ) ) ;
#808 = CARTESIAN_POINT ( 'NONE',  ( 0.04956920569949166411, -160.9696969715462274, -0.4964001826764073422 ) ) ;
#809 = DIRECTION ( 'NONE',  ( -1.224646799147353207E-16, -1.499759782661857608E-32, 1.000000000000000000 ) ) ;
#810 = CIRCLE ( 'NONE', #8403, 14.99999999999998934 ) ;
#811 = CARTESIAN_POINT ( 'NONE',  ( 27.45605056404223987, 17.16431845161426040, -2.499999999999994671 ) ) ;
#812 = AXIS2_PLACEMENT_3D ( 'NONE', #11782, #8689, #9817 ) ;
#813 = CARTESIAN_POINT ( 'NONE',  ( 42.16244658108818300, 105.4500712252157655, -2.499999999999998668 ) ) ;
#814 = DIRECTION ( 'NONE',  ( 0.6000000000000006439, -0.7999999999999996003, -0.000000000000000000 ) ) ;
#815 = AXIS2_PLACEMENT_3D ( 'NONE', #10025, #10171, #5821 ) ;
#816 = EDGE_CURVE ( 'NONE', #2083, #7574, #4917, .T. ) ;
#817 = ORIENTED_EDGE ( 'NONE', *, *, #2795, .F. ) ;
#818 = CARTESIAN_POINT ( 'NONE',  ( 16.34455450841068469, -1.870656171256066758, 2.499999999999998224 ) ) ;
#819 = FACE_OUTER_BOUND ( 'NONE', #8492, .T. ) ;
#820 = AXIS2_PLACEMENT_3D ( 'NONE', #4318, #13041, #7679 ) ;
#821 = DIRECTION ( 'NONE',  ( 1.000000000000000000, 0.000000000000000000, 0.000000000000000000 ) ) ;
#822 = VECTOR ( 'NONE', #5012, 1000.000000000000000 ) ;
#823 = ORIENTED_EDGE ( 'NONE', *, *, #10455, .T. ) ;
#824 = LINE ( 'NONE', #6347, #9737 ) ;
#825 = ORIENTED_EDGE ( 'NONE', *, *, #8248, .F. ) ;
#826 = CARTESIAN_POINT ( 'NONE',  ( 25.00000000000000355, 120.0000000000000142, -0.5000000000000000000 ) ) ;
#827 = FACE_OUTER_BOUND ( 'NONE', #12015, .T. ) ;
#828 = CARTESIAN_POINT ( 'NONE',  ( -2.733214919987291491, -81.93939393967723106, 9.473759075773607208 ) ) ;
#829 = CIRCLE ( 'NONE', #87, 20.00000000000001066 ) ;
#830 = CARTESIAN_POINT ( 'NONE',  ( 3.915768125671617028, -76.35064935075745041, 2.796074470131364453 ) ) ;
#831 = DIRECTION ( 'NONE',  ( -1.000000000000000000, 0.000000000000000000, 0.000000000000000000 ) ) ;
#832 = DIRECTION ( 'NONE',  ( -0.5999999999999999778, -0.8000000000000000444, -2.220446049250313081E-15 ) ) ;
#833 = FACE_OUTER_BOUND ( 'NONE', #4970, .T. ) ;
#834 = CARTESIAN_POINT ( 'NONE',  ( 12.99553232110413781, 77.04820039461787928, 0.000000000000000000 ) ) ;
#835 = CIRCLE ( 'NONE', #11129, 5.999999999999998224 ) ;
#836 = ORIENTED_EDGE ( 'NONE', *, *, #122, .F. ) ;
#837 = CARTESIAN_POINT ( 'NONE',  ( -8.277783874104137851, -87.06151417676248627, 4.224168635135138850 ) ) ;
#838 = ORIENTED_EDGE ( 'NONE', *, *, #9996, .T. ) ;
#839 = CYLINDRICAL_SURFACE ( 'NONE', #9881, 2.000000000000000000 ) ;
#840 = CARTESIAN_POINT ( 'NONE',  ( 39.06230589874904524, 109.5835921350012683, 7.500000000000000000 ) ) ;
#841 = LINE ( 'NONE', #11493, #7119 ) ;
#842 = CARTESIAN_POINT ( 'NONE',  ( -12.99579180576516002, -1.889935973073298747, -25.99158361153033070 ) ) ;
#843 = CARTESIAN_POINT ( 'NONE',  ( -0.1741440327402171140, -159.7354236601310618, 1.510075946869572139 ) ) ;
#844 = DIRECTION ( 'NONE',  ( -6.158143864569485777E-17, -2.736152283717910599E-16, 1.000000000000000000 ) ) ;
#845 =( BOUNDED_SURFACE ( )  B_SPLINE_SURFACE ( 3, 3, ( 
 ( #6944, #9195, #8914, #2607 ),
 ( #3860, #13219, #11084, #12361 ),
 ( #2814, #8141, #1476, #443 ),
 ( #5979, #5756, #12423, #4701 ) ),
 .UNSPECIFIED., .F., .F., .T. ) 
 B_SPLINE_SURFACE_WITH_KNOTS ( ( 4, 4 ),
 ( 4, 4 ),
 ( 0.000000000000000000, 1.000000000000000000 ),
 ( 0.000000000000000000, 1.000000000000000000 ),
 .UNSPECIFIED. ) 
 GEOMETRIC_REPRESENTATION_ITEM ( )  RATIONAL_B_SPLINE_SURFACE ( (
 ( 1.000000000000000000, 0.3333333333333334259, 0.3333333333333334259, 1.000000000000000000),
 ( 1.000000000000000000, 0.3333333333333334259, 0.3333333333333334259, 1.000000000000000000),
 ( 1.000000000000000000, 0.3333333333333334259, 0.3333333333333334259, 1.000000000000000000),
 ( 1.000000000000000000, 0.3333333333333334259, 0.3333333333333334259, 1.000000000000000000) ) ) 
 REPRESENTATION_ITEM ( '' )  SURFACE ( )  );
#846 = EDGE_LOOP ( 'NONE', ( #3292, #9316, #3361, #5959 ) ) ;
#847 = ORIENTED_EDGE ( 'NONE', *, *, #3025, .F. ) ;
#848 = DIRECTION ( 'NONE',  ( -6.158143864569485777E-17, -2.736152283717910599E-16, 1.000000000000000000 ) ) ;
#849 = VERTEX_POINT ( 'NONE', #10319 ) ;
#850 = ADVANCED_FACE ( 'NONE', ( #13445 ), #9785, .F. ) ;
#851 = LINE ( 'NONE', #5055, #5935 ) ;
#852 = EDGE_LOOP ( 'NONE', ( #11923, #5200, #8675, #11651 ) ) ;
#853 = CARTESIAN_POINT ( 'NONE',  ( -8.385254915620299343, 78.67828027274755698, -2.258796916435532892E-15 ) ) ;
#854 = ORIENTED_EDGE ( 'NONE', *, *, #10805, .F. ) ;
#855 = DIRECTION ( 'NONE',  ( 1.086108692045681373E-16, -1.448144922727572616E-16, 1.000000000000000000 ) ) ;
#856 = CARTESIAN_POINT ( 'NONE',  ( 32.50998312217522113, 0.2231948658680386610, -47.50005079999998969 ) ) ;
#857 = CARTESIAN_POINT ( 'NONE',  ( 82.09155748149851206, -71.43674177705591433, -2.500000000000000000 ) ) ;
#858 = DIRECTION ( 'NONE',  ( -6.158143864569485777E-17, -2.736152283717910599E-16, 1.000000000000000000 ) ) ;
#859 = CARTESIAN_POINT ( 'NONE',  ( -2.642019774883006988, -134.5079500460111319, 2.362135513950679666 ) ) ;
#860 = DIRECTION ( 'NONE',  ( -0.1234677578012386562, -1.701584941912606716E-18, 0.9923485843107423543 ) ) ;
#861 = ORIENTED_EDGE ( 'NONE', *, *, #13453, .F. ) ;
#862 = EDGE_LOOP ( 'NONE', ( #10905, #5451, #901, #8011 ) ) ;
#863 = VERTEX_POINT ( 'NONE', #3020 ) ;
#864 = VECTOR ( 'NONE', #910, 1000.000000000000000 ) ;
#865 = DIRECTION ( 'NONE',  ( -2.797435172181481150E-17, 1.000000000000000000, -1.765856845898762549E-18 ) ) ;
#866 = AXIS2_PLACEMENT_3D ( 'NONE', #6033, #509, #433 ) ;
#867 = EDGE_CURVE ( 'NONE', #11483, #10241, #6721, .T. ) ;
#868 = DIRECTION ( 'NONE',  ( -1.000000000000000000, 0.000000000000000000, 0.000000000000000000 ) ) ;
#869 = CARTESIAN_POINT ( 'NONE',  ( 10.00000000000000000, 92.00000000000000000, 2.500000000000000000 ) ) ;
#870 = CARTESIAN_POINT ( 'NONE',  ( 5.038813069536555389, -96.69644570957702001, 6.323701593888624295 ) ) ;
#871 = CARTESIAN_POINT ( 'NONE',  ( -25.00000000000000000, -35.00000000000000000, -7.500000000000000000 ) ) ;
#872 = ADVANCED_FACE ( 'NONE', ( #11705 ), #7390, .T. ) ;
#873 = CARTESIAN_POINT ( 'NONE',  ( 41.99999999999999289, 120.0000000000000284, -2.500000000000000000 ) ) ;
#874 = EDGE_CURVE ( 'NONE', #397, #9139, #6281, .T. ) ;
#875 = DIRECTION ( 'NONE',  ( -1.150550675996984260E-16, -1.357138225298697177E-16, 1.000000000000000000 ) ) ;
#876 = CIRCLE ( 'NONE', #4681, 5.000000000000000000 ) ;
#877 = DIRECTION ( 'NONE',  ( 1.000000000000000000, 0.000000000000000000, 0.000000000000000000 ) ) ;
#878 = CARTESIAN_POINT ( 'NONE',  ( 25.00000000000000355, 120.0000000000000284, 0.5000000000000000000 ) ) ;
#879 = CARTESIAN_POINT ( 'NONE',  ( -15.29705854078139993, 90.00000000000000000, -1.589271161308885878E-16 ) ) ;
#880 = ORIENTED_EDGE ( 'NONE', *, *, #11978, .F. ) ;
#881 = DIRECTION ( 'NONE',  ( 0.9960067511297463483, -0.08927794634716620936, 4.818676322152979407E-17 ) ) ;
#882 = CARTESIAN_POINT ( 'NONE',  ( 9.736331930512850619, -69.99978782402618549, 2.722951059031191612 ) ) ;
#883 = CARTESIAN_POINT ( 'NONE',  ( -12.88103206736694695, -118.2727272727293979, -6.757986543075753083 ) ) ;
#884 = ORIENTED_EDGE ( 'NONE', *, *, #7402, .F. ) ;
#885 = DIRECTION ( 'NONE',  ( -1.000000000000000000, 0.000000000000000000, 0.000000000000000000 ) ) ;
#886 = AXIS2_PLACEMENT_3D ( 'NONE', #6133, #5201, #13598 ) ;
#887 = VERTEX_POINT ( 'NONE', #11637 ) ;
#888 = CARTESIAN_POINT ( 'NONE',  ( -41.00000000000000000, -4.286263797015736496E-15, -10.49999999999999822 ) ) ;
#889 = CYLINDRICAL_SURFACE ( 'NONE', #8820, 15.29705854078139105 ) ;
#890 = CARTESIAN_POINT ( 'NONE',  ( 2.401759516345856493, -79.03030303050532268, 10.21173794894131248 ) ) ;
#891 = CARTESIAN_POINT ( 'NONE',  ( 2.224981447619138297, -153.6493506492904544, -4.266231359692138625 ) ) ;
#892 = EDGE_CURVE ( 'NONE', #6479, #12810, #2919, .T. ) ;
#893 = CARTESIAN_POINT ( 'NONE',  ( -37.50000000000000000, 120.0000000000000142, -2.499999999999998668 ) ) ;
#894 = CARTESIAN_POINT ( 'NONE',  ( 15.29705854078138394, 47.94714734142005597, 30.59411708156277854 ) ) ;
#895 = CARTESIAN_POINT ( 'NONE',  ( 25.00000000000000355, 120.0000000000000142, -2.500000000000000000 ) ) ;
#896 = VECTOR ( 'NONE', #3103, 1000.000000000000000 ) ;
#897 = CARTESIAN_POINT ( 'NONE',  ( 15.29705854078138749, 76.22148119144830503, 1.740418857596140842E-15 ) ) ;
#898 = AXIS2_PLACEMENT_3D ( 'NONE', #3051, #9567, #7189 ) ;
#899 = ORIENTED_EDGE ( 'NONE', *, *, #12455, .T. ) ;
#900 = AXIS2_PLACEMENT_3D ( 'NONE', #10736, #8572, #12938 ) ;
#901 = ORIENTED_EDGE ( 'NONE', *, *, #12822, .T. ) ;
#902 = CARTESIAN_POINT ( 'NONE',  ( -10.00000000000000711, 92.00000000000000000, 0.5000000000000000000 ) ) ;
#903 = CARTESIAN_POINT ( 'NONE',  ( 32.50000000000000000, 4.286263797015736496E-15, -7.500000000000000000 ) ) ;
#904 = ADVANCED_FACE ( 'NONE', ( #11438 ), #13579, .F. ) ;
#905 = CIRCLE ( 'NONE', #3346, 5.000000000000000000 ) ;
#906 = AXIS2_PLACEMENT_3D ( 'NONE', #5832, #13522, #6046 ) ;
#907 = DIRECTION ( 'NONE',  ( 0.000000000000000000, 0.000000000000000000, 1.000000000000000000 ) ) ;
#908 = DIRECTION ( 'NONE',  ( -2.797435172181481150E-17, 1.000000000000000000, -1.765856845898762549E-18 ) ) ;
#909 = CARTESIAN_POINT ( 'NONE',  ( 0.000000000000000000, 71.01020514433645303, 7.500000000000000000 ) ) ;
#910 = DIRECTION ( 'NONE',  ( -6.158143864569485777E-17, -2.736152283717910599E-16, 1.000000000000000000 ) ) ;
#911 = AXIS2_PLACEMENT_3D ( 'NONE', #11264, #11326, #1722 ) ;
#912 = ORIENTED_EDGE ( 'NONE', *, *, #660, .F. ) ;
#913 = CIRCLE ( 'NONE', #1338, 71.99999999999998579 ) ;
#914 = EDGE_LOOP ( 'NONE', ( #376, #7478 ) ) ;
#915 = CIRCLE ( 'NONE', #1137, 31.93204061526060755 ) ;
#916 = DIRECTION ( 'NONE',  ( -1.000000000000000000, 0.000000000000000000, 0.000000000000000000 ) ) ;
#917 = EDGE_LOOP ( 'NONE', ( #12551, #1766, #7020, #2213 ) ) ;
#918 = CYLINDRICAL_SURFACE ( 'NONE', #6361, 2.500000000000002220 ) ;
#919 = B_SPLINE_CURVE_WITH_KNOTS ( 'NONE', 3,
 ( #9871, #5582, #12906, #4525, #4389, #3338, #10902, #2151 ),
 .UNSPECIFIED., .F., .F.,
 ( 4, 2, 2, 4 ),
 ( 0.02189346042269462930, 0.02442701477284300177, 0.02569379194791718973, 0.02696056912299137770 ),
 .UNSPECIFIED. ) ;
#920 = ORIENTED_EDGE ( 'NONE', *, *, #9124, .T. ) ;
#921 = CARTESIAN_POINT ( 'NONE',  ( 12.99553232110413958, 77.04820039461787928, -25.99106464220826851 ) ) ;
#922 = ORIENTED_EDGE ( 'NONE', *, *, #12535, .F. ) ;
#923 = DIRECTION ( 'NONE',  ( -2.797435172181481150E-17, 1.000000000000000000, -1.765856845898762549E-18 ) ) ;
#924 = AXIS2_PLACEMENT_3D ( 'NONE', #9907, #12941, #4643 ) ;
#925 = DIRECTION ( 'NONE',  ( 0.1928999275155751925, 0.9812184353977893014, 2.891205793291787151E-16 ) ) ;
#926 = CARTESIAN_POINT ( 'NONE',  ( 13.94188849117746010, 1.893657697999892475, 2.499999999999999112 ) ) ;
#927 = CIRCLE ( 'NONE', #10546, 21.99999999999999289 ) ;
#928 = CARTESIAN_POINT ( 'NONE',  ( 22.49448184590488609, 22.22300645049884693, -2.499999999999993783 ) ) ;
#929 = DIRECTION ( 'NONE',  ( 0.000000000000000000, 0.000000000000000000, -1.000000000000000000 ) ) ;
#930 = AXIS2_PLACEMENT_3D ( 'NONE', #2671, #4852, #1475 ) ;
#931 = CARTESIAN_POINT ( 'NONE',  ( 3.452401867291364557, -108.4018358419776007, -5.656396446225017804 ) ) ;
#932 = CARTESIAN_POINT ( 'NONE',  ( 1.653273178848927024E-14, -135.0000000000000000, 0.000000000000000000 ) ) ;
#933 = ORIENTED_EDGE ( 'NONE', *, *, #12978, .T. ) ;
#934 = EDGE_LOOP ( 'NONE', ( #5830, #10072 ) ) ;
#935 = ADVANCED_FACE ( 'NONE', ( #4068 ), #5189, .T. ) ;
#936 = B_SPLINE_CURVE_WITH_KNOTS ( 'NONE', 3,
 ( #8249, #1793, #6082, #4827 ),
 .UNSPECIFIED., .F., .F.,
 ( 4, 4 ),
 ( 0.000000000000000000, 1.000000000000000000 ),
 .UNSPECIFIED. ) ;
#937 = ORIENTED_EDGE ( 'NONE', *, *, #12975, .F. ) ;
#938 = EDGE_LOOP ( 'NONE', ( #5796, #12498, #1323, #6671 ) ) ;
#939 = DIRECTION ( 'NONE',  ( 1.000000000000000000, 0.000000000000000000, 0.000000000000000000 ) ) ;
#940 = ORIENTED_EDGE ( 'NONE', *, *, #7461, .F. ) ;
#941 = DIRECTION ( 'NONE',  ( -0.000000000000000000, -0.000000000000000000, -1.000000000000000000 ) ) ;
#942 = CARTESIAN_POINT ( 'NONE',  ( 0.3822922200478666155, -101.0602069644519361, 7.519122157920856253 ) ) ;
#943 = DIRECTION ( 'NONE',  ( 1.000000000000000000, 0.000000000000000000, 0.000000000000000000 ) ) ;
#944 = CARTESIAN_POINT ( 'NONE',  ( 12.99579180576516890, 64.08350967699263379, 1.492731922528324790E-15 ) ) ;
#945 = LINE ( 'NONE', #811, #6925 ) ;
#946 = CARTESIAN_POINT ( 'NONE',  ( 26.69171018101576465, -19.44228176112429551, -2.500000000000004441 ) ) ;
#947 = DIRECTION ( 'NONE',  ( 1.000000000000000000, 0.000000000000000000, 0.000000000000000000 ) ) ;
#948 = DIRECTION ( 'NONE',  ( -1.000000000000000000, 0.000000000000000000, 0.000000000000000000 ) ) ;
#949 = ADVANCED_FACE ( 'NONE', ( #7224 ), #12480, .T. ) ;
#950 = EDGE_CURVE ( 'NONE', #6854, #11418, #8882, .T. ) ;
#951 = DIRECTION ( 'NONE',  ( -2.797435172181481150E-17, 1.000000000000000000, -1.765856845898762549E-18 ) ) ;
#952 = DIRECTION ( 'NONE',  ( 0.000000000000000000, 0.000000000000000000, 1.000000000000000000 ) ) ;
#953 = PLANE ( 'NONE',  #898 ) ;
#954 = CARTESIAN_POINT ( 'NONE',  ( -12.85867081388705202, -161.0909090911694932, -2.071848600304991628 ) ) ;
#955 = ADVANCED_FACE ( 'NONE', ( #6648 ), #3283, .T. ) ;
#956 = EDGE_LOOP ( 'NONE', ( #10577, #10149, #7801, #1791 ) ) ;
#957 = LINE ( 'NONE', #5218, #13120 ) ;
#958 = EDGE_LOOP ( 'NONE', ( #6961, #7365, #10552, #12347, #1694 ) ) ;
#959 = DIRECTION ( 'NONE',  ( 0.000000000000000000, 0.000000000000000000, 1.000000000000000000 ) ) ;
#960 = FACE_OUTER_BOUND ( 'NONE', #5437, .T. ) ;
#961 = DIRECTION ( 'NONE',  ( -0.000000000000000000, 0.000000000000000000, -1.000000000000000000 ) ) ;
#962 = CARTESIAN_POINT ( 'NONE',  ( -3.894934744997970100, -89.44155844158483148, 2.935215040339494763 ) ) ;
#963 = LINE ( 'NONE', #2075, #5370 ) ;
#964 = CARTESIAN_POINT ( 'NONE',  ( 10.69346802281034670, 49.59884612375012125, 2.619144277183853949E-15 ) ) ;
#965 = DIRECTION ( 'NONE',  ( -0.000000000000000000, -0.000000000000000000, -1.000000000000000000 ) ) ;
#966 = EDGE_CURVE ( 'NONE', #3769, #3176, #4398, .T. ) ;
#967 = CARTESIAN_POINT ( 'NONE',  ( -4.804060984082282104, 90.20500167315060480, 1.391503737930616991 ) ) ;
#968 = CIRCLE ( 'NONE', #8787, 8.385254915620292238 ) ;
#969 = EDGE_CURVE ( 'NONE', #3210, #1805, #10968, .T. ) ;
#970 = EDGE_CURVE ( 'NONE', #11470, #1977, #6576, .T. ) ;
#971 = AXIS2_PLACEMENT_3D ( 'NONE', #3341, #7616, #566 ) ;
#972 = SURFACE_STYLE_USAGE ( .BOTH. , #13448 ) ;
#973 = VERTEX_POINT ( 'NONE', #10843 ) ;
#974 = CARTESIAN_POINT ( 'NONE',  ( -12.99579180576516180, -11.31471392308272428, -25.99158361153033425 ) ) ;
#975 = DIRECTION ( 'NONE',  ( 1.000000000000000000, 1.224646799147353207E-16, 0.000000000000000000 ) ) ;
#976 = CARTESIAN_POINT ( 'NONE',  ( 15.29705854078138394, 55.48535772202409788, 30.59411708156277854 ) ) ;
#977 = CARTESIAN_POINT ( 'NONE',  ( 1.489377283214609049, -147.9547819581979979, 1.534577776538655680 ) ) ;
#978 = AXIS2_PLACEMENT_3D ( 'NONE', #10454, #11440, #9408 ) ;
#979 = EDGE_CURVE ( 'NONE', #4467, #10258, #13122, .T. ) ;
#980 = CARTESIAN_POINT ( 'NONE',  ( 15.29705854078138927, 47.94714734142005597, 1.790347283588440782E-15 ) ) ;
#981 = VECTOR ( 'NONE', #12875, 999.9999999999998863 ) ;
#982 = ORIENTED_EDGE ( 'NONE', *, *, #1139, .T. ) ;
#983 = EDGE_LOOP ( 'NONE', ( #6992, #11956, #8964, #6518 ) ) ;
#984 = EDGE_CURVE ( 'NONE', #10478, #10108, #1576, .T. ) ;
#985 = FACE_OUTER_BOUND ( 'NONE', #11435, .T. ) ;
#986 = ORIENTED_EDGE ( 'NONE', *, *, #8544, .T. ) ;
#987 = CARTESIAN_POINT ( 'NONE',  ( 10.69346802281034670, 77.87317997377837742, 1.216646543541944040E-15 ) ) ;
#988 = VERTEX_POINT ( 'NONE', #13058 ) ;
#989 = CARTESIAN_POINT ( 'NONE',  ( 15.29705854078139282, 8.361467971976981772, 1.856918518244840178E-15 ) ) ;
#990 = CIRCLE ( 'NONE', #4811, 8.385254915620297567 ) ;
#991 = CARTESIAN_POINT ( 'NONE',  ( -0.3728392436186487857, -81.93939393937360194, 10.00978956348542326 ) ) ;
#992 = DIRECTION ( 'NONE',  ( 6.158143864569485777E-17, 2.736152283717910599E-16, -1.000000000000000000 ) ) ;
#993 = CARTESIAN_POINT ( 'NONE',  ( 10.69381717166375267, 63.25855867215299355, 0.000000000000000000 ) ) ;
#994 = LINE ( 'NONE', #857, #4463 ) ;
#995 = CARTESIAN_POINT ( 'NONE',  ( -35.06230589874904524, 106.5835921350012825, -2.486789939184904430 ) ) ;
#996 = CARTESIAN_POINT ( 'NONE',  ( 10.69346802281034847, 68.44840202376897764, -21.38693604562068984 ) ) ;
#997 = CARTESIAN_POINT ( 'NONE',  ( -0.5124393331798130502, -128.8492006177044118, 4.163771180444989284 ) ) ;
#998 = DIRECTION ( 'NONE',  ( -1.000000000000000000, 0.000000000000000000, 0.000000000000000000 ) ) ;
#999 = ORIENTED_EDGE ( 'NONE', *, *, #11843, .F. ) ;
#1000 = ORIENTED_EDGE ( 'NONE', *, *, #11502, .T. ) ;
#1001 = ORIENTED_EDGE ( 'NONE', *, *, #13764, .T. ) ;
#1002 = AXIS2_PLACEMENT_3D ( 'NONE', #11272, #5952, #10357 ) ;
#1003 = CARTESIAN_POINT ( 'NONE',  ( 45.97632359910777922, 102.2167537197081657, -2.499999999999998668 ) ) ;
#1004 = ORIENTED_EDGE ( 'NONE', *, *, #10303, .F. ) ;
#1005 = CYLINDRICAL_SURFACE ( 'NONE', #9526, 15.29705854078139993 ) ;
#1006 = CARTESIAN_POINT ( 'NONE',  ( -0.8060388441294140671, -102.1876712484548335, 7.345991765615691449 ) ) ;
#1007 = DIRECTION ( 'NONE',  ( -0.9960067511297463483, 0.08927794634716618161, -4.818676322152979407E-17 ) ) ;
#1008 = DIRECTION ( 'NONE',  ( -1.000000000000000000, 0.000000000000000000, 0.000000000000000000 ) ) ;
#1009 = DIRECTION ( 'NONE',  ( -0.9960067511297463483, 0.08927794634716619548, 0.000000000000000000 ) ) ;
#1010 = AXIS2_PLACEMENT_3D ( 'NONE', #3254, #3057, #10751 ) ;
#1011 = DIRECTION ( 'NONE',  ( -0.000000000000000000, -0.000000000000000000, -1.000000000000000000 ) ) ;
#1012 = CARTESIAN_POINT ( 'NONE',  ( 25.00000000000000355, 120.0000000000000142, 0.5000000000000000000 ) ) ;
#1013 = SPHERICAL_SURFACE ( 'NONE', #5602, 5.000000000000000000 ) ;
#1014 = AXIS2_PLACEMENT_3D ( 'NONE', #10951, #11113, #1354 ) ;
#1015 = CARTESIAN_POINT ( 'NONE',  ( 12.99553232110413781, 67.62342244460847951, 0.000000000000000000 ) ) ;
#1016 =( REPRESENTATION_RELATIONSHIP ('NONE','NONE', #9450, #12318 ) REPRESENTATION_RELATIONSHIP_WITH_TRANSFORMATION ( #6084 )SHAPE_REPRESENTATION_RELATIONSHIP( ) );
#1017 = CARTESIAN_POINT ( 'NONE',  ( 34.24999999999975842, -135.0000000000000000, 0.000000000000000000 ) ) ;
#1018 = CARTESIAN_POINT ( 'NONE',  ( -28.79177319725820894, -26.24642857144861807, -4.000000000000000000 ) ) ;
#1019 = CARTESIAN_POINT ( 'NONE',  ( 47.69307742500824787, -16.90904448151677286, -2.500000000000002665 ) ) ;
#1020 = CARTESIAN_POINT ( 'NONE',  ( -20.16774360697312218, -62.63636366012922707, 2.887214123323314841 ) ) ;
#1021 = TOROIDAL_SURFACE ( 'NONE', #7490, 17.49999999999999289, 5.000000000000000000 ) ;
#1022 = ORIENTED_EDGE ( 'NONE', *, *, #13080, .F. ) ;
#1023 = LINE ( 'NONE', #5290, #2346 ) ;
#1024 = AXIS2_PLACEMENT_3D ( 'NONE', #3165, #1075, #2972 ) ;
#1025 = EDGE_LOOP ( 'NONE', ( #2026, #393, #13216, #12913 ) ) ;
#1026 = DIRECTION ( 'NONE',  ( -1.000000000000000000, 0.000000000000000000, 0.000000000000000000 ) ) ;
#1027 = AXIS2_PLACEMENT_3D ( 'NONE', #3290, #11714, #10718 ) ;
#1028 = CYLINDRICAL_SURFACE ( 'NONE', #11070, 8.385254915620292238 ) ;
#1029 = B_SPLINE_CURVE_WITH_KNOTS ( 'NONE', 3,
 ( #12936, #2255, #8632, #233 ),
 .UNSPECIFIED., .F., .F.,
 ( 4, 4 ),
 ( 0.000000000000000000, 1.000000000000000000 ),
 .UNSPECIFIED. ) ;
#1030 = FACE_BOUND ( 'NONE', #4686, .T. ) ;
#1031 = CARTESIAN_POINT ( 'NONE',  ( -12.66071438417701778, -140.5584415584565079, -5.506376209458912818 ) ) ;
#1032 = DIRECTION ( 'NONE',  ( -0.000000000000000000, -0.000000000000000000, -1.000000000000000000 ) ) ;
#1033 = DIRECTION ( 'NONE',  ( -1.000000000000000000, 0.000000000000000000, 0.000000000000000000 ) ) ;
#1034 = AXIS2_PLACEMENT_3D ( 'NONE', #5912, #7786, #12369 ) ;
#1035 = CARTESIAN_POINT ( 'NONE',  ( -15.29705854078138927, -36.87585420866476227, -1.743114418628290232E-15 ) ) ;
#1036 = DIRECTION ( 'NONE',  ( 0.000000000000000000, 0.000000000000000000, 1.000000000000000000 ) ) ;
#1037 = AXIS2_PLACEMENT_3D ( 'NONE', #4299, #2123, #12878 ) ;
#1038 = AXIS2_PLACEMENT_3D ( 'NONE', #10347, #9293, #11462 ) ;
#1039 = EDGE_LOOP ( 'NONE', ( #4656, #2047, #6993, #8729 ) ) ;
#1040 = CIRCLE ( 'NONE', #12469, 24.99999999999998934 ) ;
#1041 = EDGE_CURVE ( 'NONE', #11894, #11396, #10088, .T. ) ;
#1042 =( LENGTH_UNIT ( ) NAMED_UNIT ( * ) SI_UNIT ( .MILLI., .METRE. ) );
#1043 = ORIENTED_EDGE ( 'NONE', *, *, #4815, .T. ) ;
#1044 = FACE_OUTER_BOUND ( 'NONE', #8362, .T. ) ;
#1045 = EDGE_CURVE ( 'NONE', #1633, #1929, #12847, .T. ) ;
#1046 = CARTESIAN_POINT ( 'NONE',  ( 12.99553232110412893, 67.62342244460847951, 25.99106464220826851 ) ) ;
#1047 = CARTESIAN_POINT ( 'NONE',  ( -10.69346802281034847, 30.74929022373126841, -2.692987470725032262E-15 ) ) ;
#1048 = ADVANCED_FACE ( 'NONE', ( #10908 ), #10, .T. ) ;
#1049 = DIRECTION ( 'NONE',  ( -6.158143864569485777E-17, -2.736152283717910599E-16, 1.000000000000000000 ) ) ;
#1050 = ADVANCED_FACE ( 'NONE', ( #3213 ), #11773, .T. ) ;
#1051 = CARTESIAN_POINT ( 'NONE',  ( 0.8615837080506374424, -151.0610343063302139, 1.652123164482231843 ) ) ;
#1052 = CIRCLE ( 'NONE', #5516, 24.99999999999998934 ) ;
#1053 = FACE_OUTER_BOUND ( 'NONE', #11895, .T. ) ;
#1054 = ORIENTED_EDGE ( 'NONE', *, *, #10887, .F. ) ;
#1055 = EDGE_LOOP ( 'NONE', ( #5377, #10230, #6043, #5850 ) ) ;
#1056 = DIRECTION ( 'NONE',  ( -6.158143864569485777E-17, -2.736152283717910599E-16, 1.000000000000000000 ) ) ;
#1057 = ORIENTED_EDGE ( 'NONE', *, *, #1663, .F. ) ;
#1058 = EDGE_LOOP ( 'NONE', ( #9637, #4616, #13233, #12790 ) ) ;
#1059 = ORIENTED_EDGE ( 'NONE', *, *, #4359, .T. ) ;
#1060 = DIRECTION ( 'NONE',  ( 1.000000000000000000, 0.000000000000000000, 0.000000000000000000 ) ) ;
#1061 = CARTESIAN_POINT ( 'NONE',  ( -60.00000000000001421, 20.00000000000000000, 4.000000000000000000 ) ) ;
#1062 = FACE_OUTER_BOUND ( 'NONE', #5350, .T. ) ;
#1063 = DIRECTION ( 'NONE',  ( -1.000000000000000000, -5.171946152600901754E-17, 0.000000000000000000 ) ) ;
#1064 = EDGE_CURVE ( 'NONE', #7475, #1472, #12093, .T. ) ;
#1065 = CARTESIAN_POINT ( 'NONE',  ( -34.98870950856983342, 106.6817206552402837, -2.472621650539468696 ) ) ;
#1066 = DIRECTION ( 'NONE',  ( -1.000000000000000000, 0.000000000000000000, 0.000000000000000000 ) ) ;
#1067 = CARTESIAN_POINT ( 'NONE',  ( 5.223624298350400430, -118.2088257147582340, 1.581264552922174049 ) ) ;
#1068 = DIRECTION ( 'NONE',  ( -0.5999999999999966471, 0.8000000000000024869, 0.000000000000000000 ) ) ;
#1069 = VERTEX_POINT ( 'NONE', #9950 ) ;
#1070 = B_SPLINE_CURVE_WITH_KNOTS ( 'NONE', 3,
 ( #4019, #11528, #11726, #1079 ),
 .UNSPECIFIED., .F., .F.,
 ( 4, 4 ),
 ( 0.000000000000000000, 0.002999984648040830010 ),
 .UNSPECIFIED. ) ;
#1071 = EDGE_LOOP ( 'NONE', ( #5655, #1958, #7489, #10006 ) ) ;
#1072 = ORIENTED_EDGE ( 'NONE', *, *, #13240, .F. ) ;
#1073 = DIRECTION ( 'NONE',  ( -1.000000000000000000, 0.000000000000000000, 0.000000000000000000 ) ) ;
#1074 = ORIENTED_EDGE ( 'NONE', *, *, #3879, .T. ) ;
#1075 = DIRECTION ( 'NONE',  ( -6.158143864569485777E-17, -2.736152283717910599E-16, 1.000000000000000000 ) ) ;
#1076 = CARTESIAN_POINT ( 'NONE',  ( 4.325223352540145783, -97.40615224493882351, 6.735768676233161223 ) ) ;
#1077 = DIRECTION ( 'NONE',  ( -1.224646799147353207E-16, 1.000000000000000000, -0.000000000000000000 ) ) ;
#1078 = CARTESIAN_POINT ( 'NONE',  ( -1.024176664971890860, -142.5800865798597670, -2.358741788134935735 ) ) ;
#1079 = CARTESIAN_POINT ( 'NONE',  ( 9.736331930512850619, -69.99978782402618549, 2.722951059031191612 ) ) ;
#1080 = CARTESIAN_POINT ( 'NONE',  ( -0.08455446438426061917, -80.00111630769902149, -10.00862910738027622 ) ) ;
#1081 = DIRECTION ( 'NONE',  ( -0.000000000000000000, -0.000000000000000000, 1.000000000000000000 ) ) ;
#1082 = EDGE_CURVE ( 'NONE', #6722, #11449, #5669, .T. ) ;
#1083 = CARTESIAN_POINT ( 'NONE',  ( -9.888538082662732265, -70.78787878787531440, -1.806551902650875840 ) ) ;
#1084 = DIRECTION ( 'NONE',  ( 1.000000000000000000, 0.000000000000000000, 0.000000000000000000 ) ) ;
#1085 = DIRECTION ( 'NONE',  ( -1.000000000000000000, 0.000000000000000000, 0.000000000000000000 ) ) ;
#1086 = VECTOR ( 'NONE', #12985, 1000.000000000000000 ) ;
#1087 = CARTESIAN_POINT ( 'NONE',  ( 41.49999999999999289, 98.00000000000001421, 2.499999999999999556 ) ) ;
#1088 = CARTESIAN_POINT ( 'NONE',  ( 12.99579180576516713, 73.50828762700209040, 1.478592833246211056E-15 ) ) ;
#1089 = ORIENTED_EDGE ( 'NONE', *, *, #632, .F. ) ;
#1090 = ORIENTED_EDGE ( 'NONE', *, *, #5651, .F. ) ;
#1091 = CARTESIAN_POINT ( 'NONE',  ( -10.69381717166375800, -12.13966492792242846, -1.266741076154724095E-15 ) ) ;
#1092 = ORIENTED_EDGE ( 'NONE', *, *, #61, .F. ) ;
#1093 = CARTESIAN_POINT ( 'NONE',  ( -32.50000000000000000, -3.980102097228898626E-15, -4.000000000000000000 ) ) ;
#1094 = DIRECTION ( 'NONE',  ( -2.797435172181481150E-17, 1.000000000000000000, -1.765856845898762549E-18 ) ) ;
#1095 = CARTESIAN_POINT ( 'NONE',  ( 8.385254915620290461, 3.280056672672171381, 16.77050983124058803 ) ) ;
#1096 = FACE_OUTER_BOUND ( 'NONE', #7554, .T. ) ;
#1097 = AXIS2_PLACEMENT_3D ( 'NONE', #9065, #13450, #4710 ) ;
#1098 = CARTESIAN_POINT ( 'NONE',  ( 0.000000000000000000, 71.01020514433645303, 2.499999999999999556 ) ) ;
#1099 = CARTESIAN_POINT ( 'NONE',  ( 8.385254915620294014, 24.75422479069652582, 9.996449125125100638E-16 ) ) ;
#1100 = CARTESIAN_POINT ( 'NONE',  ( 14.20591609908153430, -14.75994833063034406, -2.500000000000004441 ) ) ;
#1101 = CARTESIAN_POINT ( 'NONE',  ( -12.99553232110414136, 77.04820039461787928, -1.863605890287647356E-15 ) ) ;
#1102 = CARTESIAN_POINT ( 'NONE',  ( -49.99999999999999289, 120.0000000000000142, 2.500000000000000000 ) ) ;
#1103 = EDGE_CURVE ( 'NONE', #769, #13399, #1351, .T. ) ;
#1104 = CIRCLE ( 'NONE', #10496, 17.49999999999999289 ) ;
#1105 = ORIENTED_EDGE ( 'NONE', *, *, #9011, .T. ) ;
#1106 = AXIS2_PLACEMENT_3D ( 'NONE', #4084, #6068, #10604 ) ;
#1107 = VERTEX_POINT ( 'NONE', #3516 ) ;
#1108 = CARTESIAN_POINT ( 'NONE',  ( 34.99999999999958789, 1.104930248025249758E-13, -2.499999999999999112 ) ) ;
#1109 = DIRECTION ( 'NONE',  ( 1.000000000000000000, 0.000000000000000000, 0.000000000000000000 ) ) ;
#1110 = AXIS2_PLACEMENT_3D ( 'NONE', #13074, #1328, #3491 ) ;
#1111 = CARTESIAN_POINT ( 'NONE',  ( 35.22727272727274084, 140.0412797136805523, 7.500000000000000000 ) ) ;
#1112 = SURFACE_STYLE_USAGE ( .BOTH. , #4254 ) ;
#1113 = DIRECTION ( 'NONE',  ( -0.000000000000000000, -0.000000000000000000, -1.000000000000000000 ) ) ;
#1114 = B_SPLINE_CURVE_WITH_KNOTS ( 'NONE', 3,
 ( #9543, #8352, #1834, #4988 ),
 .UNSPECIFIED., .F., .F.,
 ( 4, 4 ),
 ( 0.000000000000000000, 1.000000000000000000 ),
 .UNSPECIFIED. ) ;
#1115 = CIRCLE ( 'NONE', #6929, 8.385254915620292238 ) ;
#1116 = CARTESIAN_POINT ( 'NONE',  ( -15.29705854078138749, 10.24803554138234496, -1.909542505269288522E-15 ) ) ;
#1117 = ORIENTED_EDGE ( 'NONE', *, *, #5565, .F. ) ;
#1118 = EDGE_CURVE ( 'NONE', #2729, #11470, #9632, .T. ) ;
#1119 = ORIENTED_EDGE ( 'NONE', *, *, #6804, .F. ) ;
#1120 = EDGE_CURVE ( 'NONE', #9797, #887, #7165, .T. ) ;
#1121 = AXIS2_PLACEMENT_3D ( 'NONE', #5344, #1273, #9629 ) ;
#1122 = EDGE_CURVE ( 'NONE', #7574, #1929, #10739, .T. ) ;
#1123 = ADVANCED_FACE ( 'NONE', ( #3312 ), #7797, .F. ) ;
#1124 = CIRCLE ( 'NONE', #8726, 15.29705854078139637 ) ;
#1125 = AXIS2_PLACEMENT_3D ( 'NONE', #11875, #4574, #6551 ) ;
#1126 = CARTESIAN_POINT ( 'NONE',  ( 10.00000000000000000, 92.00000000000000000, -0.5000000000000000000 ) ) ;
#1127 = ORIENTED_EDGE ( 'NONE', *, *, #11633, .T. ) ;
#1128 = CARTESIAN_POINT ( 'NONE',  ( 10.00000000000000000, 92.00000000000000000, -0.5000000000000000000 ) ) ;
#1129 = CARTESIAN_POINT ( 'NONE',  ( -10.00000000000000711, 99.99999999999994316, 0.5000000000000000000 ) ) ;
#1130 =( NAMED_UNIT ( * ) SI_UNIT ( $, .STERADIAN. ) SOLID_ANGLE_UNIT ( ) );
#1131 = CARTESIAN_POINT ( 'NONE',  ( 39.31777158827904373, 101.3359913474316585, -2.434761661425244306 ) ) ;
#1132 = DIRECTION ( 'NONE',  ( 1.000000000000000000, 0.000000000000000000, 0.000000000000000000 ) ) ;
#1133 = CARTESIAN_POINT ( 'NONE',  ( -7.323500324365400438, -96.14321736266329310, -3.508298222391299959 ) ) ;
#1134 = LINE ( 'NONE', #8488, #10413 ) ;
#1135 = EDGE_LOOP ( 'NONE', ( #10525, #11632, #5422, #13706 ) ) ;
#1136 = ADVANCED_FACE ( 'NONE', ( #7729 ), #4429, .F. ) ;
#1137 = AXIS2_PLACEMENT_3D ( 'NONE', #9842, #9775, #5630 ) ;
#1138 = ORIENTED_EDGE ( 'NONE', *, *, #7758, .T. ) ;
#1139 = EDGE_CURVE ( 'NONE', #8182, #10177, #6498, .T. ) ;
#1140 = ORIENTED_EDGE ( 'NONE', *, *, #4608, .F. ) ;
#1141 = EDGE_CURVE ( 'NONE', #2083, #1633, #9870, .T. ) ;
#1142 = ADVANCED_FACE ( 'NONE', ( #12014 ), #6615, .F. ) ;
#1143 = CYLINDRICAL_SURFACE ( 'NONE', #11409, 15.29705854078139815 ) ;
#1144 = CIRCLE ( 'NONE', #8981, 25.50000000002549783 ) ;
#1145 = CARTESIAN_POINT ( 'NONE',  ( -42.16244658108818300, 105.4500712252157655, 7.500000000000000000 ) ) ;
#1146 = VERTEX_POINT ( 'NONE', #12161 ) ;
#1147 = CARTESIAN_POINT ( 'NONE',  ( 34.99999999999958789, 1.104930248025249758E-13, -2.499999999999999112 ) ) ;
#1148 = CARTESIAN_POINT ( 'NONE',  ( 15.29705854078138927, 38.52236939141059935, -30.59411708156276788 ) ) ;
#1149 = CARTESIAN_POINT ( 'NONE',  ( 1.436028440950094742, -80.32363832966076700, -10.00441251861082748 ) ) ;
#1150 = CIRCLE ( 'NONE', #496, 20.00000000000000000 ) ;
#1151 = DIRECTION ( 'NONE',  ( 0.000000000000000000, 1.000000000000000000, 0.000000000000000000 ) ) ;
#1152 = CIRCLE ( 'NONE', #8747, 8.385254915620290461 ) ;
#1153 = CARTESIAN_POINT ( 'NONE',  ( 50.89489709276795537, 9.943703908052052398, -2.499999999999994671 ) ) ;
#1154 = CARTESIAN_POINT ( 'NONE',  ( 0.6059849270565064172, -166.5454544424325718, -5.665245052758470123 ) ) ;
#1155 = CARTESIAN_POINT ( 'NONE',  ( -9.991007172155491389, -71.90909090909036649, -2.111483349789142760 ) ) ;
#1156 = DIRECTION ( 'NONE',  ( -1.000000000000000000, 0.000000000000000000, 0.000000000000000000 ) ) ;
#1157 = DIRECTION ( 'NONE',  ( -6.158143864569485777E-17, -2.736152283717910599E-16, 1.000000000000000000 ) ) ;
#1158 = ORIENTED_EDGE ( 'NONE', *, *, #4130, .T. ) ;
#1159 = CIRCLE ( 'NONE', #3378, 15.29705854078139282 ) ;
#1160 = CARTESIAN_POINT ( 'NONE',  ( -15.29705854078139637, 74.33491362204294717, -3.876297867647458896E-15 ) ) ;
#1161 = EDGE_CURVE ( 'NONE', #3518, #4148, #7840, .T. ) ;
#1162 = DIRECTION ( 'NONE',  ( -1.000000000000000000, 0.000000000000000000, 0.000000000000000000 ) ) ;
#1163 = CARTESIAN_POINT ( 'NONE',  ( 14.00979921278056040, -2.538005261501627086, -2.500000000000000888 ) ) ;
#1164 = EDGE_LOOP ( 'NONE', ( #8091, #8679, #11162, #3980 ) ) ;
#1165 = DIRECTION ( 'NONE',  ( -6.158143864569485777E-17, -2.736152283717910599E-16, 1.000000000000000000 ) ) ;
#1166 = ORIENTED_EDGE ( 'NONE', *, *, #9006, .F. ) ;
#1167 = CARTESIAN_POINT ( 'NONE',  ( -25.00000000000000355, 120.0000000000000142, -2.499999999999998668 ) ) ;
#1168 = DIRECTION ( 'NONE',  ( 0.9960067511297463483, -0.08927794634716620936, 4.626175998653454121E-17 ) ) ;
#1169 = LINE ( 'NONE', #9923, #5204 ) ;
#1170 = CIRCLE ( 'NONE', #2960, 50.00000000000001421 ) ;
#1171 = CARTESIAN_POINT ( 'NONE',  ( -10.69381717166375623, -2.714886977913000710, -1.300026693482923793E-15 ) ) ;
#1172 = CARTESIAN_POINT ( 'NONE',  ( 12.99579180576517246, 26.38439787695498495, -25.99158361153033070 ) ) ;
#1173 = CARTESIAN_POINT ( 'NONE',  ( 40.81228451836346238, 100.6358150620708187, 0.6381026355483961909 ) ) ;
#1174 = DIRECTION ( 'NONE',  ( -0.2228746399763467390, 0.9748471135800802490, 2.409338161076489210E-16 ) ) ;
#1175 = VERTEX_POINT ( 'NONE', #6831 ) ;
#1176 = VERTEX_POINT ( 'NONE', #1427 ) ;
#1177 = SURFACE_STYLE_FILL_AREA ( #6501 ) ;
#1178 = VERTEX_POINT ( 'NONE', #4654 ) ;
#1179 = CARTESIAN_POINT ( 'NONE',  ( -10.00000000000000711, 139.9999999999999716, -0.5000000000000000000 ) ) ;
#1180 = DIRECTION ( 'NONE',  ( 0.9960067511297463483, -0.08927794634716620936, 4.626175998653454121E-17 ) ) ;
#1181 = DIRECTION ( 'NONE',  ( 0.000000000000000000, 1.000000000000000000, 0.000000000000000000 ) ) ;
#1182 = CARTESIAN_POINT ( 'NONE',  ( 23.75221630157310315, -98.98132178242397572, 7.500000000000000000 ) ) ;
#1183 = DIRECTION ( 'NONE',  ( -1.000000000000000000, 0.000000000000000000, 0.000000000000000000 ) ) ;
#1184 = EDGE_LOOP ( 'NONE', ( #6080, #7628, #1059, #324 ) ) ;
#1185 = ORIENTED_EDGE ( 'NONE', *, *, #4539, .F. ) ;
#1186 = CIRCLE ( 'NONE', #2980, 5.000000000000000000 ) ;
#1187 = AXIS2_PLACEMENT_3D ( 'NONE', #3327, #7602, #3393 ) ;
#1188 = ORIENTED_EDGE ( 'NONE', *, *, #12808, .T. ) ;
#1189 = ORIENTED_EDGE ( 'NONE', *, *, #6708, .T. ) ;
#1190 = DIRECTION ( 'NONE',  ( -1.000000000000000000, 0.000000000000000000, 0.000000000000000000 ) ) ;
#1191 = EDGE_CURVE ( 'NONE', #4658, #10763, #8941, .T. ) ;
#1192 = DIRECTION ( 'NONE',  ( 2.668805347656626185E-16, -1.000000000000000000, -0.000000000000000000 ) ) ;
#1193 = ADVANCED_FACE ( 'NONE', ( #2400 ), #10537, .F. ) ;
#1194 = CARTESIAN_POINT ( 'NONE',  ( -7.273479275674047173, -73.48250329347293075, -7.060675431679237057 ) ) ;
#1195 = CARTESIAN_POINT ( 'NONE',  ( -24.99999999999999289, -99.86284836912238916, 4.640101051368102247 ) ) ;
#1196 = CARTESIAN_POINT ( 'NONE',  ( -38.89115197531750567, 101.6687180808697519, -2.500000000000000000 ) ) ;
#1197 = CARTESIAN_POINT ( 'NONE',  ( -15.29705854078139637, 64.91013567203349055, -1.146220074446778111E-16 ) ) ;
#1198 = FACE_OUTER_BOUND ( 'NONE', #4757, .T. ) ;
#1199 = ORIENTED_EDGE ( 'NONE', *, *, #3503, .F. ) ;
#1200 = EDGE_LOOP ( 'NONE', ( #6060, #8837, #10579, #545 ) ) ;
#1201 = ORIENTED_EDGE ( 'NONE', *, *, #6512, .T. ) ;
#1202 = AXIS2_PLACEMENT_3D ( 'NONE', #6544, #2391, #9908 ) ;
#1203 = DIRECTION ( 'NONE',  ( 1.000000000000000000, 0.000000000000000000, 0.000000000000000000 ) ) ;
#1204 = CARTESIAN_POINT ( 'NONE',  ( -33.99999999999999289, 108.0000000000000142, 0.5000000000000000000 ) ) ;
#1205 = ORIENTED_EDGE ( 'NONE', *, *, #8589, .T. ) ;
#1206 = CARTESIAN_POINT ( 'NONE',  ( 35.65577094119244350, -20.24578327824959345, -2.500000000000003997 ) ) ;
#1207 =( NAMED_UNIT ( * ) PLANE_ANGLE_UNIT ( ) SI_UNIT ( $, .RADIAN. ) );
#1208 = CIRCLE ( 'NONE', #93, 42.00000000000001421 ) ;
#1209 = CARTESIAN_POINT ( 'NONE',  ( -12.99553232110414136, 58.19864449459907974, -3.303875580016498200E-15 ) ) ;
#1210 = ADVANCED_FACE ( 'NONE', ( #8649 ), #5552, .T. ) ;
#1211 = CARTESIAN_POINT ( 'NONE',  ( 43.14708730495711819, 24.16350488746832781, 7.806255641895631925E-15 ) ) ;
#1212 = CARTESIAN_POINT ( 'NONE',  ( -12.99579180576516713, 45.23395377697384134, -1.751278857619846450E-15 ) ) ;
#1213 = CARTESIAN_POINT ( 'NONE',  ( 1.066429238991517314, -168.0000000000001421, -0.4719413927851733859 ) ) ;
#1214 = EDGE_CURVE ( 'NONE', #4795, #6682, #915, .T. ) ;
#1215 = CARTESIAN_POINT ( 'NONE',  ( -9.601587402597671073, -70.78787878788241983, -2.975959431766524776 ) ) ;
#1216 = CARTESIAN_POINT ( 'NONE',  ( -25.00000000000000355, 120.0000000000000142, -0.5000000000000000000 ) ) ;
#1217 = EDGE_CURVE ( 'NONE', #1501, #10825, #13244, .T. ) ;
#1218 = DIRECTION ( 'NONE',  ( 0.000000000000000000, 1.000000000000000000, 0.000000000000000000 ) ) ;
#1219 = EDGE_CURVE ( 'NONE', #3278, #2483, #11318, .T. ) ;
#1220 = ORIENTED_EDGE ( 'NONE', *, *, #4700, .F. ) ;
#1221 = CARTESIAN_POINT ( 'NONE',  ( 35.08961652778860696, 18.74878582411816197, -2.499999999999993783 ) ) ;
#1222 = EDGE_LOOP ( 'NONE', ( #13644, #9404, #50, #12785 ) ) ;
#1223 = VECTOR ( 'NONE', #10636, 1000.000000000000000 ) ;
#1224 = FACE_OUTER_BOUND ( 'NONE', #917, .T. ) ;
#1225 = DIRECTION ( 'NONE',  ( -1.000000000000000000, 0.000000000000000000, 0.000000000000000000 ) ) ;
#1226 = VERTEX_POINT ( 'NONE', #6896 ) ;
#1227 = AXIS2_PLACEMENT_3D ( 'NONE', #6619, #9995, #5635 ) ;
#1228 = LINE ( 'NONE', #3519, #7961 ) ;
#1229 = VERTEX_POINT ( 'NONE', #11110 ) ;
#1230 = DIRECTION ( 'NONE',  ( -0.8907235428302473501, 0.4545454545454531425, 0.000000000000000000 ) ) ;
#1231 = CARTESIAN_POINT ( 'NONE',  ( 8.385254915620294014, 3.280056672672171381, 2.053795118489800793E-15 ) ) ;
#1232 = EDGE_CURVE ( 'NONE', #4529, #4849, #6504, .T. ) ;
#1233 = VECTOR ( 'NONE', #7883, 1000.000000000000114 ) ;
#1234 = B_SPLINE_CURVE_WITH_KNOTS ( 'NONE', 3,
 ( #10165, #572, #4533, #8815 ),
 .UNSPECIFIED., .F., .F.,
 ( 4, 4 ),
 ( 0.000000000000000000, 1.000000000000000000 ),
 .UNSPECIFIED. ) ;
#1235 = DIRECTION ( 'NONE',  ( 0.000000000000000000, 0.000000000000000000, -1.000000000000000000 ) ) ;
#1236 = CARTESIAN_POINT ( 'NONE',  ( 39.06230589874905235, 109.5835921350012683, 7.500000000000000000 ) ) ;
#1237 = CYLINDRICAL_SURFACE ( 'NONE', #11778, 8.385254915620292238 ) ;
#1238 = ADVANCED_FACE ( 'NONE', ( #1643 ), #3580, .T. ) ;
#1239 = CARTESIAN_POINT ( 'NONE',  ( -39.06230589874905235, 109.5835921350012683, -7.500000000000000000 ) ) ;
#1240 = CARTESIAN_POINT ( 'NONE',  ( 12.99579180576515647, 16.95961992694555676, 25.99158361153032359 ) ) ;
#1241 = VECTOR ( 'NONE', #9971, 1000.000000000000000 ) ;
#1242 = DIRECTION ( 'NONE',  ( -2.797435172181481150E-17, 1.000000000000000000, -1.765856845898762549E-18 ) ) ;
#1243 = ORIENTED_EDGE ( 'NONE', *, *, #7794, .F. ) ;
#1244 = VERTEX_POINT ( 'NONE', #1713 ) ;
#1245 = ORIENTED_EDGE ( 'NONE', *, *, #1141, .F. ) ;
#1246 = AXIS2_PLACEMENT_3D ( 'NONE', #4641, #1628, #9135 ) ;
#1247 = DIRECTION ( 'NONE',  ( 6.158143864569485777E-17, 2.736152283717910599E-16, -1.000000000000000000 ) ) ;
#1248 = DIRECTION ( 'NONE',  ( 0.4206864060305147146, -0.9072061219927525233, -2.409338161076489703E-16 ) ) ;
#1249 = PRODUCT_DEFINITION_FORMATION_WITH_SPECIFIED_SOURCE ( 'ANY', '', #10016, .NOT_KNOWN. ) ;
#1250 = VECTOR ( 'NONE', #11018, 1000.000000000000000 ) ;
#1251 = DIRECTION ( 'NONE',  ( -2.797435172181481150E-17, 1.000000000000000000, -1.765856845898762549E-18 ) ) ;
#1252 = UNCERTAINTY_MEASURE_WITH_UNIT (LENGTH_MEASURE( 1.000000000000000082E-05 ), #1376, 'distance_accuracy_value', 'NONE');
#1253 = CARTESIAN_POINT ( 'NONE',  ( 12.99553232110413958, 11.07475474455194053, 3.182987412051231773E-15 ) ) ;
#1254 = EDGE_LOOP ( 'NONE', ( #12301, #6976, #1516, #6221, #12477, #13271, #4805, #4411 ) ) ;
#1255 = ORIENTED_EDGE ( 'NONE', *, *, #7784, .F. ) ;
#1256 = ORIENTED_EDGE ( 'NONE', *, *, #354, .F. ) ;
#1257 = VERTEX_POINT ( 'NONE', #3812 ) ;
#1258 = CARTESIAN_POINT ( 'NONE',  ( -18.54049621773915746, -20.00000000000000000, -7.500000000000000000 ) ) ;
#1259 = DIRECTION ( 'NONE',  ( -1.000000000000000000, 0.000000000000000000, 0.000000000000000000 ) ) ;
#1260 = CARTESIAN_POINT ( 'NONE',  ( -1.964926745380544348, -77.94210580202374672, -9.914063068206223406 ) ) ;
#1261 = CARTESIAN_POINT ( 'NONE',  ( 2.974540731479519701E-17, -1.063309978032472847, 1.877653204021102445E-18 ) ) ;
#1262 = CARTESIAN_POINT ( 'NONE',  ( 4.130090007162176668, 90.90347248489021581, -2.819710018450384048 ) ) ;
#1263 = DIRECTION ( 'NONE',  ( -0.000000000000000000, -0.000000000000000000, -1.000000000000000000 ) ) ;
#1264 = ORIENTED_EDGE ( 'NONE', *, *, #10289, .T. ) ;
#1265 = ORIENTED_EDGE ( 'NONE', *, *, #114, .T. ) ;
#1266 = CIRCLE ( 'NONE', #10884, 10.00000000000000178 ) ;
#1267 = CARTESIAN_POINT ( 'NONE',  ( -4.317896099768527840, 91.66241202089433671, 2.521541801375117853 ) ) ;
#1268 = EDGE_LOOP ( 'NONE', ( #3247, #638, #10126, #9802 ) ) ;
#1269 = DIRECTION ( 'NONE',  ( 0.4226182617407009401, -0.9063077870366491595, -0.000000000000000000 ) ) ;
#1270 = DIRECTION ( 'NONE',  ( 0.000000000000000000, 0.000000000000000000, 1.000000000000000000 ) ) ;
#1271 = FACE_OUTER_BOUND ( 'NONE', #11973, .T. ) ;
#1272 = CARTESIAN_POINT ( 'NONE',  ( 21.51985683731163945, -13.03114504999992995, -2.500000000000004441 ) ) ;
#1273 = DIRECTION ( 'NONE',  ( -0.000000000000000000, -0.000000000000000000, -1.000000000000000000 ) ) ;
#1274 = LINE ( 'NONE', #7718, #3945 ) ;
#1275 = FACE_OUTER_BOUND ( 'NONE', #7688, .T. ) ;
#1276 = DIRECTION ( 'NONE',  ( -1.000000000000000000, 0.000000000000000000, 0.000000000000000000 ) ) ;
#1277 =( BOUNDED_SURFACE ( )  B_SPLINE_SURFACE ( 3, 3, ( 
 ( #10028, #438, #8065, #644 ),
 ( #3786, #8982, #13288, #1539 ),
 ( #3637, #4909, #7011, #5823 ),
 ( #11291, #9186, #7928, #12211 ) ),
 .UNSPECIFIED., .F., .F., .F. ) 
 B_SPLINE_SURFACE_WITH_KNOTS ( ( 4, 4 ),
 ( 4, 4 ),
 ( 0.000000000000000000, 1.000000000000000000 ),
 ( 0.000000000000000000, 1.000000000000000000 ),
 .UNSPECIFIED. ) 
 GEOMETRIC_REPRESENTATION_ITEM ( )  RATIONAL_B_SPLINE_SURFACE ( (
 ( 1.000000000000000000, 0.3333333333333334259, 0.3333333333333334259, 1.000000000000000000),
 ( 1.000000000000000000, 0.3333333333333334259, 0.3333333333333334259, 1.000000000000000000),
 ( 1.000000000000000000, 0.3333333333333334259, 0.3333333333333334259, 1.000000000000000000),
 ( 1.000000000000000000, 0.3333333333333334259, 0.3333333333333334259, 1.000000000000000000) ) ) 
 REPRESENTATION_ITEM ( '' )  SURFACE ( )  );
#1278 = VERTEX_POINT ( 'NONE', #13536 ) ;
#1279 = EDGE_CURVE ( 'NONE', #12858, #420, #13718, .T. ) ;
#1280 = DIRECTION ( 'NONE',  ( -1.000000000000000000, 0.000000000000000000, 0.000000000000000000 ) ) ;
#1281 = CARTESIAN_POINT ( 'NONE',  ( -12.99579180576517068, 73.50828762700209040, -3.329728542850656599E-15 ) ) ;
#1282 = ORIENTED_EDGE ( 'NONE', *, *, #6005, .F. ) ;
#1283 = EDGE_CURVE ( 'NONE', #11234, #8652, #11660, .T. ) ;
#1284 = EDGE_CURVE ( 'NONE', #4658, #12645, #13017, .T. ) ;
#1285 = CARTESIAN_POINT ( 'NONE',  ( -24.99999999999999645, -99.15310334213022259, -0.4257687054510825297 ) ) ;
#1286 = CARTESIAN_POINT ( 'NONE',  ( 10.00000000000000000, 98.00000000000000000, 0.5000000000000000000 ) ) ;
#1287 = ADVANCED_FACE ( 'NONE', ( #8164 ), #7175, .T. ) ;
#1288 = ORIENTED_EDGE ( 'NONE', *, *, #12701, .F. ) ;
#1289 = DIRECTION ( 'NONE',  ( -0.000000000000000000, -0.000000000000000000, -1.000000000000000000 ) ) ;
#1290 = ORIENTED_EDGE ( 'NONE', *, *, #4117, .T. ) ;
#1291 = EDGE_CURVE ( 'NONE', #7693, #12930, #4483, .T. ) ;
#1292 = DIRECTION ( 'NONE',  ( -0.000000000000000000, -0.000000000000000000, -1.000000000000000000 ) ) ;
#1293 = CARTESIAN_POINT ( 'NONE',  ( -10.69381717166375978, 25.55944687211528787, 21.38763434332751245 ) ) ;
#1294 = DIRECTION ( 'NONE',  ( 1.000000000000000000, 0.000000000000000000, 0.000000000000000000 ) ) ;
#1295 = CARTESIAN_POINT ( 'NONE',  ( -8.385254915620292238, -22.36966495935058319, 3.950162600893091522E-17 ) ) ;
#1296 = CARTESIAN_POINT ( 'NONE',  ( 35.20000000000002416, 106.4000000000000199, 2.500000000000000000 ) ) ;
#1297 = CARTESIAN_POINT ( 'NONE',  ( 12.99579180576517601, -30.16426982310158067, 3.183050967463144563E-15 ) ) ;
#1298 = CARTESIAN_POINT ( 'NONE',  ( -25.00000000000000355, 120.0000000000000142, 7.500000000000000000 ) ) ;
#1299 = DIRECTION ( 'NONE',  ( -1.000000000000000000, -5.171946152600901754E-17, 0.000000000000000000 ) ) ;
#1300 = DIRECTION ( 'NONE',  ( -0.000000000000000000, -0.000000000000000000, -1.000000000000000000 ) ) ;
#1301 = CIRCLE ( 'NONE', #4422, 15.70031846811053455 ) ;
#1302 = AXIS2_PLACEMENT_3D ( 'NONE', #287, #3633, #1682 ) ;
#1303 = ADVANCED_FACE ( 'NONE', ( #3952 ), #8974, .T. ) ;
#1304 = DIRECTION ( 'NONE',  ( -1.000000000000000000, 0.000000000000000000, 0.000000000000000000 ) ) ;
#1305 = ORIENTED_EDGE ( 'NONE', *, *, #1729, .F. ) ;
#1306 = CARTESIAN_POINT ( 'NONE',  ( -10.00000000000000711, 139.9999999999999716, 2.500000000000000000 ) ) ;
#1307 = CARTESIAN_POINT ( 'NONE',  ( 15.29705854078138927, 90.00000000000000000, 1.714422261702872766E-15 ) ) ;
#1308 = CARTESIAN_POINT ( 'NONE',  ( 8.385254915620294014, -15.56949922734665570, 1.052073721316228694E-15 ) ) ;
#1309 = CARTESIAN_POINT ( 'NONE',  ( 7.679260624019852705E-16, -27.45107625865536605, 4.847467093863555185E-17 ) ) ;
#1310 = ORIENTED_EDGE ( 'NONE', *, *, #12273, .F. ) ;
#1311 = DIRECTION ( 'NONE',  ( 6.158143864569485777E-17, 2.736152283717910599E-16, -1.000000000000000000 ) ) ;
#1312 = ADVANCED_FACE ( 'NONE', ( #11256 ), #4731, .T. ) ;
#1313 = CIRCLE ( 'NONE', #12980, 2.000000000000003997 ) ;
#1314 = ORIENTED_EDGE ( 'NONE', *, *, #12004, .T. ) ;
#1315 = VERTEX_POINT ( 'NONE', #8228 ) ;
#1316 = DIRECTION ( 'NONE',  ( -2.797435172181481150E-17, 1.000000000000000000, -1.765856845898762549E-18 ) ) ;
#1317 = CARTESIAN_POINT ( 'NONE',  ( 48.00000000000000000, 120.0000000000000284, -0.5000000000000000000 ) ) ;
#1318 = FACE_BOUND ( 'NONE', #1621, .T. ) ;
#1319 = DIRECTION ( 'NONE',  ( 1.000000000000000000, 0.000000000000000000, 0.000000000000000000 ) ) ;
#1320 = CARTESIAN_POINT ( 'NONE',  ( 3.629742700906665842, 90.29727615934677942, -3.441963681523289686 ) ) ;
#1321 = CARTESIAN_POINT ( 'NONE',  ( -7.363455934862510155, -88.30281729203618113, 5.335658674741773133 ) ) ;
#1322 = DIRECTION ( 'NONE',  ( 0.9960067511297464593, -0.08927794634716622324, 3.401418580343279473E-17 ) ) ;
#1323 = ORIENTED_EDGE ( 'NONE', *, *, #10531, .T. ) ;
#1324 = CIRCLE ( 'NONE', #6265, 2.000000000000003997 ) ;
#1325 = ORIENTED_EDGE ( 'NONE', *, *, #13518, .F. ) ;
#1326 = ORIENTED_EDGE ( 'NONE', *, *, #12213, .F. ) ;
#1327 = VECTOR ( 'NONE', #9078, 1000.000000000000000 ) ;
#1328 = DIRECTION ( 'NONE',  ( -6.158143864569485777E-17, -2.736152283717910599E-16, 1.000000000000000000 ) ) ;
#1329 = CARTESIAN_POINT ( 'NONE',  ( 40.87368016229836343, -22.78235879061915625, 2.499999999999993783 ) ) ;
#1330 = ORIENTED_EDGE ( 'NONE', *, *, #1895, .T. ) ;
#1331 = DIRECTION ( 'NONE',  ( 2.797435172181480534E-17, -1.000000000000000000, 1.765856845898762164E-18 ) ) ;
#1332 =( NAMED_UNIT ( * ) PLANE_ANGLE_UNIT ( ) SI_UNIT ( $, .RADIAN. ) );
#1333 = CARTESIAN_POINT ( 'NONE',  ( 10.69381717166374912, 34.98422482212468054, 21.38763434332751245 ) ) ;
#1334 = CARTESIAN_POINT ( 'NONE',  ( 12.99579180576517068, 7.534841976936129448, -25.99158361153032359 ) ) ;
#1335 = VECTOR ( 'NONE', #12650, 1000.000000000000000 ) ;
#1336 = CARTESIAN_POINT ( 'NONE',  ( 34.99999999999958789, 1.091249486606660213E-13, 2.500000000000000000 ) ) ;
#1337 = CARTESIAN_POINT ( 'NONE',  ( -0.5048931899935213963, -158.0606060608750170, -1.721373026808497686 ) ) ;
#1338 = AXIS2_PLACEMENT_3D ( 'NONE', #7809, #6559, #6766 ) ;
#1339 = DIRECTION ( 'NONE',  ( -1.000000000000000000, 0.000000000000000000, 0.000000000000000000 ) ) ;
#1340 = EDGE_CURVE ( 'NONE', #6463, #2032, #1803, .T. ) ;
#1341 = CARTESIAN_POINT ( 'NONE',  ( -39.00000000000000000, -4.776122516674677878E-15, -8.499999999999998224 ) ) ;
#1342 = CARTESIAN_POINT ( 'NONE',  ( 6.999999999999992006, 144.0000000000000284, -2.500000000000000000 ) ) ;
#1343 = ORIENTED_EDGE ( 'NONE', *, *, #7796, .T. ) ;
#1344 = ORIENTED_EDGE ( 'NONE', *, *, #970, .T. ) ;
#1345 = CARTESIAN_POINT ( 'NONE',  ( -35.00000000000000000, -4.286263797015736496E-15, -7.500000000000000000 ) ) ;
#1346 = CARTESIAN_POINT ( 'NONE',  ( -10.69381717166375090, 72.68333662216240043, -21.38763434332750890 ) ) ;
#1347 = AXIS2_PLACEMENT_3D ( 'NONE', #10348, #1507, #478 ) ;
#1348 = FACE_BOUND ( 'NONE', #3706, .T. ) ;
#1349 = CIRCLE ( 'NONE', #3140, 25.50418395392908977 ) ;
#1350 = DIRECTION ( 'NONE',  ( 1.000000000000000000, 2.797435172181480534E-17, -0.000000000000000000 ) ) ;
#1351 = LINE ( 'NONE', #10878, #7831 ) ;
#1352 = ORIENTED_EDGE ( 'NONE', *, *, #406, .F. ) ;
#1353 = EDGE_LOOP ( 'NONE', ( #10331, #161, #8745, #6168 ) ) ;
#1354 = DIRECTION ( 'NONE',  ( -1.000000000000000000, 0.000000000000000000, 0.000000000000000000 ) ) ;
#1355 = VERTEX_POINT ( 'NONE', #1774 ) ;
#1356 = LINE ( 'NONE', #4508, #9291 ) ;
#1357 = CYLINDRICAL_SURFACE ( 'NONE', #12995, 18.74900000001875000 ) ;
#1358 = CARTESIAN_POINT ( 'NONE',  ( 12.99579180576516535, 45.23395377697384134, 1.521010101092551666E-15 ) ) ;
#1359 = DIRECTION ( 'NONE',  ( 0.000000000000000000, 0.000000000000000000, 1.000000000000000000 ) ) ;
#1360 = ADVANCED_FACE ( 'NONE', ( #4804 ), #4937, .T. ) ;
#1361 = CIRCLE ( 'NONE', #924, 77.49999999999998579 ) ;
#1362 = CARTESIAN_POINT ( 'NONE',  ( -1.077638310512993291E-15, 38.52236939141059935, -6.802498971006334016E-17 ) ) ;
#1363 = CARTESIAN_POINT ( 'NONE',  ( -12.99553232110413958, 67.62342244460847951, -1.830320272959447658E-15 ) ) ;
#1364 = EDGE_CURVE ( 'NONE', #3469, #6698, #2244, .T. ) ;
#1365 = SHAPE_REPRESENTATION ( 'Threaded Steel Worm Screw Spindle', ( #8193 ), #11552 ) ;
#1366 = CARTESIAN_POINT ( 'NONE',  ( 40.73187278757659868, 100.6589795836331831, 1.037129925556720789 ) ) ;
#1367 = LINE ( 'NONE', #10689, #5432 ) ;
#1368 = AXIS2_PLACEMENT_3D ( 'NONE', #5270, #9352, #4013 ) ;
#1369 = CARTESIAN_POINT ( 'NONE',  ( 8.385254915620292238, 15.32944684068712782, 2.053795118489800004E-15 ) ) ;
#1370 = EDGE_CURVE ( 'NONE', #2025, #13844, #9640, .T. ) ;
#1371 = DIRECTION ( 'NONE',  ( -0.000000000000000000, -0.000000000000000000, -1.000000000000000000 ) ) ;
#1372 = ORIENTED_EDGE ( 'NONE', *, *, #3276, .F. ) ;
#1373 = EDGE_LOOP ( 'NONE', ( #9014, #4066, #10422, #13661 ) ) ;
#1374 = FACE_OUTER_BOUND ( 'NONE', #10512, .T. ) ;
#1375 = CIRCLE ( 'NONE', #13736, 4.999999999999997335 ) ;
#1376 =( LENGTH_UNIT ( ) NAMED_UNIT ( * ) SI_UNIT ( .MILLI., .METRE. ) );
#1377 = ORIENTED_EDGE ( 'NONE', *, *, #1772, .T. ) ;
#1378 = CYLINDRICAL_SURFACE ( 'NONE', #10821, 9.000000000008999024 ) ;
#1379 = ADVANCED_FACE ( 'NONE', ( #6065 ), #9145, .T. ) ;
#1380 = CARTESIAN_POINT ( 'NONE',  ( -37.50000000000000711, -4.286263797015736496E-15, 7.500000000000000000 ) ) ;
#1381 = DIRECTION ( 'NONE',  ( 1.000000000000000000, 0.000000000000000000, 0.000000000000000000 ) ) ;
#1382 = DIRECTION ( 'NONE',  ( -2.797435172181481150E-17, 1.000000000000000000, -1.765856845898762549E-18 ) ) ;
#1383 = CARTESIAN_POINT ( 'NONE',  ( 4.789632241632986620, -77.94522257074953586, 8.921723374081109270 ) ) ;
#1384 = ADVANCED_FACE ( 'NONE', ( #9399 ), #12637, .T. ) ;
#1385 = ORIENTED_EDGE ( 'NONE', *, *, #11158, .T. ) ;
#1386 = EDGE_CURVE ( 'NONE', #12240, #1176, #4981, .T. ) ;
#1387 = PRODUCT ( 'Central Body Frame & Collar', 'Central Body Frame & Collar', '', ( #270 ) ) ;
#1388 = ORIENTED_EDGE ( 'NONE', *, *, #4419, .F. ) ;
#1389 = ORIENTED_EDGE ( 'NONE', *, *, #4269, .F. ) ;
#1390 = ORIENTED_EDGE ( 'NONE', *, *, #7706, .F. ) ;
#1391 = DIRECTION ( 'NONE',  ( -1.000000000000000000, 0.000000000000000000, 0.000000000000000000 ) ) ;
#1392 = DIRECTION ( 'NONE',  ( 1.000000000000000000, 6.938893903907227392E-16, 0.000000000000000000 ) ) ;
#1393 = CARTESIAN_POINT ( 'NONE',  ( 34.99999999999958789, 1.063887963769481123E-13, 12.50000000000000000 ) ) ;
#1394 = ADVANCED_FACE ( 'NONE', ( #6182 ), #3012, .T. ) ;
#1395 = CARTESIAN_POINT ( 'NONE',  ( 43.63403238902020576, 20.33700654369049587, -2.499999999999992895 ) ) ;
#1396 = CARTESIAN_POINT ( 'NONE',  ( -34.31346379765673049, 108.0181378390412732, 1.328939170454191521 ) ) ;
#1397 = CARTESIAN_POINT ( 'NONE',  ( 43.29712336220986657, 19.44704974301885159, 2.500000000000005773 ) ) ;
#1398 = CARTESIAN_POINT ( 'NONE',  ( -3.521118371085406373, -100.8219657368393030, -6.686088967780647430 ) ) ;
#1399 = CARTESIAN_POINT ( 'NONE',  ( 22.00000000000000355, -34.99999999999999289, 7.500000000000000000 ) ) ;
#1400 = EDGE_LOOP ( 'NONE', ( #12032, #9944, #11231, #11351, #351 ) ) ;
#1401 = EDGE_CURVE ( 'NONE', #4911, #12400, #10094, .T. ) ;
#1402 = CIRCLE ( 'NONE', #3195, 67.49999999999997158 ) ;
#1403 = ORIENTED_EDGE ( 'NONE', *, *, #9175, .T. ) ;
#1404 = AXIS2_PLACEMENT_3D ( 'NONE', #13762, #9455, #1944 ) ;
#1405 = ADVANCED_FACE ( 'NONE', ( #4448 ), #2501, .T. ) ;
#1406 = CARTESIAN_POINT ( 'NONE',  ( 155.9864723944028810, -111.6214737678657087, 2.500000000000000000 ) ) ;
#1407 = VERTEX_POINT ( 'NONE', #7746 ) ;
#1408 = DIRECTION ( 'NONE',  ( -0.8000000000000008216, 0.5999999999999988676, 0.000000000000000000 ) ) ;
#1409 = CARTESIAN_POINT ( 'NONE',  ( 0.000000000000000000, 0.000000000000000000, 0.000000000000000000 ) ) ;
#1410 = CARTESIAN_POINT ( 'NONE',  ( 12.99553232110413781, 58.19864449459907974, 1.506840924385250240E-15 ) ) ;
#1411 = DIRECTION ( 'NONE',  ( -1.000000000000000000, 0.000000000000000000, 0.000000000000000000 ) ) ;
#1412 = AXIS2_PLACEMENT_3D ( 'NONE', #9958, #4403, #11982 ) ;
#1413 = DIRECTION ( 'NONE',  ( -0.000000000000000000, -0.000000000000000000, -1.000000000000000000 ) ) ;
#1414 = CARTESIAN_POINT ( 'NONE',  ( 8.385254915620297567, -15.56949922734665748, -16.77050983124058803 ) ) ;
#1415 = CARTESIAN_POINT ( 'NONE',  ( 4.278103086407295308, -97.41991341990937769, 7.774081346648461732 ) ) ;
#1416 = CARTESIAN_POINT ( 'NONE',  ( -10.00000000000000711, 139.9999999999999716, 2.500000000000000000 ) ) ;
#1417 = CARTESIAN_POINT ( 'NONE',  ( 15.29705854078138927, -18.02629830864593785, 30.59411708156278564 ) ) ;
#1418 = DIRECTION ( 'NONE',  ( -0.000000000000000000, -0.000000000000000000, -1.000000000000000000 ) ) ;
#1419 = VERTEX_POINT ( 'NONE', #12031 ) ;
#1420 = AXIS2_PLACEMENT_3D ( 'NONE', #4195, #5059, #13652 ) ;
#1421 = VERTEX_POINT ( 'NONE', #6775 ) ;
#1422 = ORIENTED_EDGE ( 'NONE', *, *, #9090, .F. ) ;
#1423 = CIRCLE ( 'NONE', #7924, 10.00000000000000178 ) ;
#1424 = CARTESIAN_POINT ( 'NONE',  ( 10.00000000000000000, 90.00000000000000000, 0.5000000000000000000 ) ) ;
#1425 = DIRECTION ( 'NONE',  ( -0.000000000000000000, -0.000000000000000000, -1.000000000000000000 ) ) ;
#1426 = DIRECTION ( 'NONE',  ( -0.000000000000000000, -0.000000000000000000, -1.000000000000000000 ) ) ;
#1427 = CARTESIAN_POINT ( 'NONE',  ( 15.29705854078138749, 47.94714734142005597, 1.790347283588440388E-15 ) ) ;
#1428 = EDGE_LOOP ( 'NONE', ( #10008, #3383, #8004, #1403 ) ) ;
#1429 = ORIENTED_EDGE ( 'NONE', *, *, #9258, .T. ) ;
#1430 = DIRECTION ( 'NONE',  ( 0.4545454545454531425, 0.8907235428302472391, 0.000000000000000000 ) ) ;
#1431 = ORIENTED_EDGE ( 'NONE', *, *, #3497, .F. ) ;
#1432 = DIRECTION ( 'NONE',  ( -1.000000000000000000, 0.000000000000000000, 0.000000000000000000 ) ) ;
#1433 = CARTESIAN_POINT ( 'NONE',  ( 12.99579180576516357, 16.95961992694555676, 0.000000000000000000 ) ) ;
#1434 = CIRCLE ( 'NONE', #6806, 3.999999999999996447 ) ;
#1435 = CARTESIAN_POINT ( 'NONE',  ( 34.50080218526777287, 107.5336849384755737, -2.002074976903565062 ) ) ;
#1436 = FACE_OUTER_BOUND ( 'NONE', #12588, .T. ) ;
#1437 = CARTESIAN_POINT ( 'NONE',  ( -4.259889090956146873, -78.36053271697988976, -9.185913463276904167 ) ) ;
#1438 = CARTESIAN_POINT ( 'NONE',  ( 15.29705854078139460, -29.33764382806072746, 30.59411708156279985 ) ) ;
#1439 = CARTESIAN_POINT ( 'NONE',  ( -8.385254915620295790, -34.41905512736551032, 6.077912412602530076E-17 ) ) ;
#1440 = DIRECTION ( 'NONE',  ( -1.000000000000000000, 0.000000000000000000, 0.000000000000000000 ) ) ;
#1441 = DIRECTION ( 'NONE',  ( -0.000000000000000000, -0.000000000000000000, -1.000000000000000000 ) ) ;
#1442 = ORIENTED_EDGE ( 'NONE', *, *, #8928, .F. ) ;
#1443 = VECTOR ( 'NONE', #13173, 1000.000000000000000 ) ;
#1444 = EDGE_CURVE ( 'NONE', #2799, #3806, #8730, .T. ) ;
#1445 = AXIS2_PLACEMENT_3D ( 'NONE', #4826, #13624, #10423 ) ;
#1446 = ORIENTED_EDGE ( 'NONE', *, *, #13055, .T. ) ;
#1447 = CARTESIAN_POINT ( 'NONE',  ( -2.237684797877293663E-15, 79.99058638175036151, -1.412519245696701158E-16 ) ) ;
#1448 = EDGE_LOOP ( 'NONE', ( #11783, #1558, #7098, #2655 ) ) ;
#1449 =( BOUNDED_SURFACE ( )  B_SPLINE_SURFACE ( 3, 3, ( 
 ( #10572, #12754, #9589, #5369 ),
 ( #13838, #9463, #8464, #7414 ),
 ( #7543, #6503, #1046, #6234 ),
 ( #8337, #8402, #9660, #11691 ) ),
 .UNSPECIFIED., .F., .F., .T. ) 
 B_SPLINE_SURFACE_WITH_KNOTS ( ( 4, 4 ),
 ( 4, 4 ),
 ( 0.000000000000000000, 1.000000000000000000 ),
 ( 0.000000000000000000, 1.000000000000000000 ),
 .UNSPECIFIED. ) 
 GEOMETRIC_REPRESENTATION_ITEM ( )  RATIONAL_B_SPLINE_SURFACE ( (
 ( 1.000000000000000000, 0.3333333333333334259, 0.3333333333333334259, 1.000000000000000000),
 ( 1.000000000000000000, 0.3333333333333334259, 0.3333333333333334259, 1.000000000000000000),
 ( 1.000000000000000000, 0.3333333333333334259, 0.3333333333333334259, 1.000000000000000000),
 ( 1.000000000000000000, 0.3333333333333334259, 0.3333333333333334259, 1.000000000000000000) ) ) 
 REPRESENTATION_ITEM ( '' )  SURFACE ( )  );
#1450 = DIRECTION ( 'NONE',  ( -0.000000000000000000, -0.000000000000000000, -1.000000000000000000 ) ) ;
#1451 = DIRECTION ( 'NONE',  ( 0.000000000000000000, 0.000000000000000000, 1.000000000000000000 ) ) ;
#1452 = CARTESIAN_POINT ( 'NONE',  ( 10.11144057928414242, -69.99977036137985920, -0.2534939170199681513 ) ) ;
#1453 = CIRCLE ( 'NONE', #2584, 5.000000000000000000 ) ;
#1454 = ORIENTED_EDGE ( 'NONE', *, *, #5490, .F. ) ;
#1455 = ORIENTED_EDGE ( 'NONE', *, *, #6677, .F. ) ;
#1456 = ORIENTED_EDGE ( 'NONE', *, *, #4730, .T. ) ;
#1457 = EDGE_CURVE ( 'NONE', #2229, #11958, #5249, .T. ) ;
#1458 = EDGE_CURVE ( 'NONE', #9642, #2246, #1349, .T. ) ;
#1459 = EDGE_LOOP ( 'NONE', ( #3631, #4186, #3330, #12674 ) ) ;
#1460 = VERTEX_POINT ( 'NONE', #11700 ) ;
#1461 = STYLED_ITEM ( 'NONE', ( #12222 ), #5559 ) ;
#1462 = EDGE_LOOP ( 'NONE', ( #2845, #13234, #8779, #12885 ) ) ;
#1463 = EDGE_CURVE ( 'NONE', #9210, #11257, #4951, .T. ) ;
#1464 = AXIS2_PLACEMENT_3D ( 'NONE', #932, #5068, #998 ) ;
#1465 = EDGE_CURVE ( 'NONE', #3209, #7690, #13263, .T. ) ;
#1466 = DIRECTION ( 'NONE',  ( -0.000000000000000000, -0.000000000000000000, -1.000000000000000000 ) ) ;
#1467 = CARTESIAN_POINT ( 'NONE',  ( 34.99999999999958789, 1.104930248025249758E-13, -2.499999999999999112 ) ) ;
#1468 = CARTESIAN_POINT ( 'NONE',  ( -34.25812584745450096, 108.1980041606223040, -0.6234894336158697259 ) ) ;
#1469 = CARTESIAN_POINT ( 'NONE',  ( 32.05482125692310547, -25.32934902781011743, -6.505213034913026604E-15 ) ) ;
#1470 = CARTESIAN_POINT ( 'NONE',  ( 22.84091969677297485, -17.29701610032388359, -2.500000000000004441 ) ) ;
#1471 = AXIS2_PLACEMENT_3D ( 'NONE', #642, #2138, #2806 ) ;
#1472 = VERTEX_POINT ( 'NONE', #9159 ) ;
#1473 = VERTEX_POINT ( 'NONE', #13266 ) ;
#1474 = MECHANICAL_DESIGN_GEOMETRIC_PRESENTATION_REPRESENTATION (  '', ( #5507 ), #12915 ) ;
#1475 = DIRECTION ( 'NONE',  ( 0.9960067511297464593, -0.08927794634716622324, 3.401418580343279473E-17 ) ) ;
#1476 = CARTESIAN_POINT ( 'NONE',  ( 12.99553232110413958, -26.62435705548576692, 25.99106464220828983 ) ) ;
#1477 = CARTESIAN_POINT ( 'NONE',  ( 8.152362820469006621, -73.18181818182262077, 5.943141306424061021 ) ) ;
#1478 = VERTEX_POINT ( 'NONE', #1591 ) ;
#1479 = CARTESIAN_POINT ( 'NONE',  ( 8.385254915620292238, 90.00000000000000000, 8.679704431140114636E-16 ) ) ;
#1480 = FILL_AREA_STYLE ('',( #4347 ) ) ;
#1481 = CARTESIAN_POINT ( 'NONE',  ( 55.99165482216006495, 2.525950835318802934, 2.500000000000002220 ) ) ;
#1482 = ADVANCED_FACE ( 'NONE', ( #3900 ), #7121, .T. ) ;
#1483 = DIRECTION ( 'NONE',  ( -1.000000000000000000, 0.000000000000000000, 0.000000000000000000 ) ) ;
#1484 = CARTESIAN_POINT ( 'NONE',  ( -15.29705854078139282, 46.06057977201469100, -2.036022158066717581E-15 ) ) ;
#1485 = FACE_OUTER_BOUND ( 'NONE', #145, .T. ) ;
#1486 = CARTESIAN_POINT ( 'NONE',  ( 3.913402758210908772, -81.93939393942487470, -9.205743832022209361 ) ) ;
#1487 = DIRECTION ( 'NONE',  ( -1.000000000000000000, 0.000000000000000000, 0.000000000000000000 ) ) ;
#1488 = CARTESIAN_POINT ( 'NONE',  ( 15.18222645069203303, -16.04698886238941924, 4.000000000000000000 ) ) ;
#1489 = CARTESIAN_POINT ( 'NONE',  ( 8.385254915620294014, 78.67828027274755698, 8.868043070384791430E-16 ) ) ;
#1490 = ORIENTED_EDGE ( 'NONE', *, *, #11940, .F. ) ;
#1491 = ORIENTED_EDGE ( 'NONE', *, *, #11278, .F. ) ;
#1492 = TOROIDAL_SURFACE ( 'NONE', #5294, 71.99999999999998579, 2.000000000000000000 ) ;
#1493 = CARTESIAN_POINT ( 'NONE',  ( 1.661059338047568001, -148.6780715075996966, -1.248219484669665924 ) ) ;
#1494 = ORIENTED_EDGE ( 'NONE', *, *, #725, .F. ) ;
#1495 = CARTESIAN_POINT ( 'NONE',  ( -6.036583442707799563, -95.60204248688987150, -5.530378780570661235 ) ) ;
#1496 = CARTESIAN_POINT ( 'NONE',  ( 2.008006476061143353, -80.00378950643523979, 9.910921260988354575 ) ) ;
#1497 = DIRECTION ( 'NONE',  ( -1.000000000000000000, -2.797435172181480534E-17, 0.000000000000000000 ) ) ;
#1498 = DIRECTION ( 'NONE',  ( 0.8907235428302464619, -0.4545454545454548079, 4.944508929129155689E-15 ) ) ;
#1499 = EDGE_LOOP ( 'NONE', ( #11784, #2877, #786, #13460, #13369 ) ) ;
#1500 = FACE_OUTER_BOUND ( 'NONE', #11636, .T. ) ;
#1501 = VERTEX_POINT ( 'NONE', #1787 ) ;
#1502 = CARTESIAN_POINT ( 'NONE',  ( 22.42156014662059249, -97.00000000000000000, 7.500000000000000000 ) ) ;
#1503 = EDGE_CURVE ( 'NONE', #3971, #1662, #10328, .T. ) ;
#1504 = LINE ( 'NONE', #4249, #11680 ) ;
#1505 = CARTESIAN_POINT ( 'NONE',  ( -35.00000000000000000, -4.286263797015736496E-15, 7.500000000000000000 ) ) ;
#1506 = DIRECTION ( 'NONE',  ( 0.000000000000000000, 0.000000000000000000, 1.000000000000000000 ) ) ;
#1507 = DIRECTION ( 'NONE',  ( 0.5999999999999999778, -0.8000000000000000444, -2.220446049250313081E-15 ) ) ;
#1508 = DIRECTION ( 'NONE',  ( -0.000000000000000000, -0.000000000000000000, -1.000000000000000000 ) ) ;
#1509 = CARTESIAN_POINT ( 'NONE',  ( -39.99999999999999289, 100.0000000000000000, 2.500000000000000000 ) ) ;
#1510 = CARTESIAN_POINT ( 'NONE',  ( -8.385254915620297567, -6.144721277337256815, -2.041332847496538735E-15 ) ) ;
#1511 = DIRECTION ( 'NONE',  ( 0.000000000000000000, 0.000000000000000000, 1.000000000000000000 ) ) ;
#1512 = CARTESIAN_POINT ( 'NONE',  ( 8.385254915620290461, 53.02855864072483882, 9.722760835075755586E-16 ) ) ;
#1513 = CIRCLE ( 'NONE', #5438, 25.50000000002549783 ) ;
#1514 = ORIENTED_EDGE ( 'NONE', *, *, #11143, .F. ) ;
#1515 = CARTESIAN_POINT ( 'NONE',  ( 4.208314830452973609, -157.8181818182845007, 0.6624707635749896850 ) ) ;
#1516 = ORIENTED_EDGE ( 'NONE', *, *, #7775, .T. ) ;
#1517 = CARTESIAN_POINT ( 'NONE',  ( -2.517691654963332357E-15, 90.00000000000000000, -1.589271161308885878E-16 ) ) ;
#1518 = ITEM_DEFINED_TRANSFORMATION ( 'NONE', 'NONE', #11557,  #8193 ) ;
#1519 = EDGE_LOOP ( 'NONE', ( #5605, #7612, #13308, #225, #6231, #6509, #5414, #5521, #11851, #10379 ) ) ;
#1520 = FACE_OUTER_BOUND ( 'NONE', #11031, .T. ) ;
#1521 = CARTESIAN_POINT ( 'NONE',  ( -39.06230589874905235, 109.5835921350012825, 2.499999999999999556 ) ) ;
#1522 = CARTESIAN_POINT ( 'NONE',  ( -8.385254915620297567, -34.41905512736551032, -9.053393109928500416E-16 ) ) ;
#1523 = ADVANCED_FACE ( 'NONE', ( #7899 ), #11140, .F. ) ;
#1524 = UNCERTAINTY_MEASURE_WITH_UNIT (LENGTH_MEASURE( 1.000000000000000082E-05 ), #2490, 'distance_accuracy_value', 'NONE');
#1525 = CARTESIAN_POINT ( 'NONE',  ( 25.00000000000000355, 120.0000000000000142, 0.5000000000000000000 ) ) ;
#1526 = B_SPLINE_CURVE_WITH_KNOTS ( 'NONE', 3,
 ( #1439, #481, #5716, #8954 ),
 .UNSPECIFIED., .F., .F.,
 ( 4, 4 ),
 ( 0.000000000000000000, 1.000000000000000000 ),
 .UNSPECIFIED. ) ;
#1527 = AXIS2_PLACEMENT_3D ( 'NONE', #13455, #4995, #3801 ) ;
#1528 = EDGE_LOOP ( 'NONE', ( #12574, #10244, #8782, #6113 ) ) ;
#1529 = AXIS2_PLACEMENT_3D ( 'NONE', #5524, #10912, #4542 ) ;
#1530 = CARTESIAN_POINT ( 'NONE',  ( -45.97632359910779343, 102.2167537197081799, 7.500000000000000000 ) ) ;
#1531 = LINE ( 'NONE', #5671, #12811 ) ;
#1532 = TOROIDAL_SURFACE ( 'NONE', #8693, 16.99999999999998934, 2.000000000000000000 ) ;
#1533 = CARTESIAN_POINT ( 'NONE',  ( 12.99553232110413781, 77.04820039461787928, 3.182987412051231773E-15 ) ) ;
#1534 = DIRECTION ( 'NONE',  ( 1.000000000000000000, 0.000000000000000000, 0.000000000000000000 ) ) ;
#1535 = AXIS2_PLACEMENT_3D ( 'NONE', #11860, #12937, #4416 ) ;
#1536 = CARTESIAN_POINT ( 'NONE',  ( -34.37544226909923850, 107.8407100838017385, 1.642507177281961050 ) ) ;
#1537 = CARTESIAN_POINT ( 'NONE',  ( 5.492103586168583185, -85.98458891577695340, -7.620002978679659478 ) ) ;
#1538 = EDGE_CURVE ( 'NONE', #11754, #750, #7410, .T. ) ;
#1539 = CARTESIAN_POINT ( 'NONE',  ( -12.99579180576516535, 16.95961992694555676, -3.214849374574138845E-15 ) ) ;
#1540 = EDGE_CURVE ( 'NONE', #3748, #6776, #5380, .T. ) ;
#1541 = ORIENTED_EDGE ( 'NONE', *, *, #4175, .T. ) ;
#1542 = EDGE_LOOP ( 'NONE', ( #8607, #8080, #6527, #11183 ) ) ;
#1543 = EDGE_CURVE ( 'NONE', #2454, #8513, #7588, .T. ) ;
#1544 = CIRCLE ( 'NONE', #5570, 14.99999999999999112 ) ;
#1545 = VERTEX_POINT ( 'NONE', #8855 ) ;
#1546 = CARTESIAN_POINT ( 'NONE',  ( 8.385254915620294014, -24.99427717735608212, 1.068716529980328543E-15 ) ) ;
#1547 = CARTESIAN_POINT ( 'NONE',  ( -23.75056915604791286, -98.97863401284405427, 7.500000000000000000 ) ) ;
#1548 = EDGE_LOOP ( 'NONE', ( #2270, #11697, #4778, #6657 ) ) ;
#1549 = CARTESIAN_POINT ( 'NONE',  ( 7.273479296210343392, -73.48250327241889579, 7.060675410516041417 ) ) ;
#1550 = DIRECTION ( 'NONE',  ( -2.797435172181481150E-17, 1.000000000000000000, -1.765856845898762549E-18 ) ) ;
#1551 = B_SPLINE_CURVE_WITH_KNOTS ( 'NONE', 3,
 ( #7248, #5282, #11532, #9365, #1925, #6213, #6407, #10608 ),
 .UNSPECIFIED., .F., .F.,
 ( 4, 2, 2, 4 ),
 ( 0.02696056912299137770, 0.02949568642151915651, 0.03076324507078304765, 0.03203080372004693532 ),
 .UNSPECIFIED. ) ;
#1552 = FACE_OUTER_BOUND ( 'NONE', #10987, .T. ) ;
#1553 = CARTESIAN_POINT ( 'NONE',  ( -0.4173931308523584627, -102.5454545454544615, 7.668730708677045982 ) ) ;
#1554 = DIRECTION ( 'NONE',  ( 1.000000000000000000, 0.000000000000000000, 0.000000000000000000 ) ) ;
#1555 = AXIS2_PLACEMENT_3D ( 'NONE', #329, #13101, #3459 ) ;
#1556 = DIRECTION ( 'NONE',  ( -6.158143864569485777E-17, -2.736152283717910599E-16, 1.000000000000000000 ) ) ;
#1557 = VERTEX_POINT ( 'NONE', #4427 ) ;
#1558 = ORIENTED_EDGE ( 'NONE', *, *, #9619, .F. ) ;
#1559 = AXIS2_PLACEMENT_3D ( 'NONE', #3456, #10956, #8717 ) ;
#1560 = ORIENTED_EDGE ( 'NONE', *, *, #3191, .F. ) ;
#1561 = CARTESIAN_POINT ( 'NONE',  ( 14.79219767565757770, 6.218900627562692129, -2.499999999999999112 ) ) ;
#1562 = ORIENTED_EDGE ( 'NONE', *, *, #3110, .T. ) ;
#1563 = ADVANCED_FACE ( 'NONE', ( #1348, #3447 ), #9839, .F. ) ;
#1564 = EDGE_CURVE ( 'NONE', #4257, #11572, #2193, .T. ) ;
#1565 = CARTESIAN_POINT ( 'NONE',  ( 6.060518735590991746, -109.8459309627911864, -2.257746733285272089 ) ) ;
#1566 = DIRECTION ( 'NONE',  ( 1.000000000000000000, 0.000000000000000000, 0.000000000000000000 ) ) ;
#1567 = CARTESIAN_POINT ( 'NONE',  ( -15.29705854078138927, 29.09759144140119957, -5.138218104596347907E-17 ) ) ;
#1568 = AXIS2_PLACEMENT_3D ( 'NONE', #4156, #7447, #8306 ) ;
#1569 = DIRECTION ( 'NONE',  ( -0.08715574274765883200, 0.9961946980917454342, 0.000000000000000000 ) ) ;
#1570 = EDGE_LOOP ( 'NONE', ( #12242, #620, #13076, #12492 ) ) ;
#1571 = ORIENTED_EDGE ( 'NONE', *, *, #3141, .T. ) ;
#1572 = FACE_OUTER_BOUND ( 'NONE', #13487, .T. ) ;
#1573 = ORIENTED_EDGE ( 'NONE', *, *, #5943, .T. ) ;
#1574 = LINE ( 'NONE', #1776, #7953 ) ;
#1575 = AXIS2_PLACEMENT_3D ( 'NONE', #9277, #13660, #13796 ) ;
#1576 = CIRCLE ( 'NONE', #9419, 8.385254915620294014 ) ;
#1577 = DIRECTION ( 'NONE',  ( 0.000000000000000000, 0.000000000000000000, 1.000000000000000000 ) ) ;
#1578 = CARTESIAN_POINT ( 'NONE',  ( 1.387778780781445676E-14, -135.0000000000000000, 0.000000000000000000 ) ) ;
#1579 = CARTESIAN_POINT ( 'NONE',  ( 35.00000000000000000, 4.286263797015736496E-15, 7.500000000000000000 ) ) ;
#1580 = CARTESIAN_POINT ( 'NONE',  ( -40.50666510048448288, 100.7305537260640307, -1.531269357928749963 ) ) ;
#1581 = DIRECTION ( 'NONE',  ( -6.158143864569485777E-17, -2.736152283717910599E-16, 1.000000000000000000 ) ) ;
#1582 = PLANE ( 'NONE',  #2090 ) ;
#1583 = VECTOR ( 'NONE', #8845, 1000.000000000000000 ) ;
#1584 = CYLINDRICAL_SURFACE ( 'NONE', #5114, 9.000000000008999024 ) ;
#1585 = ADVANCED_FACE ( 'NONE', ( #6678 ), #13166, .T. ) ;
#1586 = AXIS2_PLACEMENT_3D ( 'NONE', #13102, #4376, #9715 ) ;
#1587 = VERTEX_POINT ( 'NONE', #11107 ) ;
#1588 = AXIS2_PLACEMENT_3D ( 'NONE', #13019, #2479, #12948 ) ;
#1589 = CARTESIAN_POINT ( 'NONE',  ( 3.288118420601234604, 90.13403546913524167, 3.770150660886109950 ) ) ;
#1590 = ORIENTED_EDGE ( 'NONE', *, *, #1191, .T. ) ;
#1591 = CARTESIAN_POINT ( 'NONE',  ( 31.81818181818183433, 133.3608531424536920, 0.5000000000000000000 ) ) ;
#1592 = VERTEX_POINT ( 'NONE', #5777 ) ;
#1593 = DIRECTION ( 'NONE',  ( 0.000000000000000000, 1.000000000000000000, 0.000000000000000000 ) ) ;
#1594 = CARTESIAN_POINT ( 'NONE',  ( -24.99999999999998934, -100.0000000000000000, 7.500000000000000000 ) ) ;
#1595 = STYLED_ITEM ( 'NONE', ( #6768 ), #7994 ) ;
#1596 = DIRECTION ( 'NONE',  ( 0.000000000000000000, 0.000000000000000000, -1.000000000000000000 ) ) ;
#1597 = CARTESIAN_POINT ( 'NONE',  ( 0.7140975576127237545, -124.8181818181821825, -13.04184819563892539 ) ) ;
#1598 = AXIS2_PLACEMENT_3D ( 'NONE', #2233, #6519, #152 ) ;
#1599 = AXIS2_PLACEMENT_3D ( 'NONE', #518, #12281, #372 ) ;
#1600 = CARTESIAN_POINT ( 'NONE',  ( -1.552166912326615374E-15, 55.48535772202409078, -9.797919878057798703E-17 ) ) ;
#1601 = CARTESIAN_POINT ( 'NONE',  ( -25.00000000000000355, 120.0000000000000284, 0.5000000000000000000 ) ) ;
#1602 = CARTESIAN_POINT ( 'NONE',  ( 25.00000000000000355, 120.0000000000000142, -2.500000000000000000 ) ) ;
#1603 = CARTESIAN_POINT ( 'NONE',  ( -12.97449437267217931, -39.59556244224027211, 25.94898874534434796 ) ) ;
#1604 = ORIENTED_EDGE ( 'NONE', *, *, #8953, .F. ) ;
#1605 = EDGE_LOOP ( 'NONE', ( #2349, #69, #5334, #6879, #8263, #11647 ) ) ;
#1606 = AXIS2_PLACEMENT_3D ( 'NONE', #6003, #7042, #13605 ) ;
#1607 = CARTESIAN_POINT ( 'NONE',  ( 34.99999999999958789, 1.091249486606660213E-13, 2.500000000000000000 ) ) ;
#1608 = EDGE_LOOP ( 'NONE', ( #6442, #1785, #12436, #12671 ) ) ;
#1609 = CARTESIAN_POINT ( 'NONE',  ( 15.29705854078139105, -36.87585420866476227, 1.980000072520086583E-15 ) ) ;
#1610 = CYLINDRICAL_SURFACE ( 'NONE', #5111, 4.999999999999997335 ) ;
#1611 = CARTESIAN_POINT ( 'NONE',  ( 37.49001687782395464, -0.2231948658678050423, -2.499999999999997335 ) ) ;
#1612 = MECHANICAL_DESIGN_GEOMETRIC_PRESENTATION_REPRESENTATION (  '', ( #10127 ), #11476 ) ;
#1613 = CARTESIAN_POINT ( 'NONE',  ( -2.517691654963332357E-15, 90.00000000000000000, -1.589271161308885878E-16 ) ) ;
#1614 = CARTESIAN_POINT ( 'NONE',  ( 4.934221198804287667, -99.30322515911785786, 5.966777793213275061 ) ) ;
#1615 = CARTESIAN_POINT ( 'NONE',  ( 8.385254915620295790, 50.40394642271930081, -16.77050983124058803 ) ) ;
#1616 = ORIENTED_EDGE ( 'NONE', *, *, #13052, .F. ) ;
#1617 = ORIENTED_EDGE ( 'NONE', *, *, #2561, .T. ) ;
#1618 = CARTESIAN_POINT ( 'NONE',  ( -10.69346802281034847, -6.949821576306442594, -1.285027358575335329E-15 ) ) ;
#1619 = DIRECTION ( 'NONE',  ( 1.000000000000000000, 0.000000000000000000, 0.000000000000000000 ) ) ;
#1620 = CARTESIAN_POINT ( 'NONE',  ( 0.9052951019204806826, -80.99999999999998579, 10.12030223674823581 ) ) ;
#1621 = EDGE_LOOP ( 'NONE', ( #13498, #11507 ) ) ;
#1622 = FACE_OUTER_BOUND ( 'NONE', #13090, .T. ) ;
#1623 = SHAPE_REPRESENTATION_RELATIONSHIP ( 'NONE' , 'NONE' ,  #3787, #5559 ) ;
#1624 = FACE_OUTER_BOUND ( 'NONE', #6612, .T. ) ;
#1625 = DIRECTION ( 'NONE',  ( -1.000000000000000000, 0.000000000000000000, 0.000000000000000000 ) ) ;
#1626 = CARTESIAN_POINT ( 'NONE',  ( -10.69346802281034670, -16.37459952631584059, -2.593420296013165014E-15 ) ) ;
#1627 = CARTESIAN_POINT ( 'NONE',  ( 9.841394828004627726, -91.60173160174092288, 2.396245945945958411 ) ) ;
#1628 = DIRECTION ( 'NONE',  ( -6.158143864569485777E-17, -2.736152283717910599E-16, 1.000000000000000000 ) ) ;
#1629 = CARTESIAN_POINT ( 'NONE',  ( -15.29705854078138927, 19.67281349139174296, -3.473937238186366113E-17 ) ) ;
#1630 = AXIS2_PLACEMENT_3D ( 'NONE', #59, #7473, #10758 ) ;
#1631 = DIRECTION ( 'NONE',  ( -1.000000000000000000, 0.000000000000000000, 0.000000000000000000 ) ) ;
#1632 = EDGE_LOOP ( 'NONE', ( #12045, #10879, #4615, #10703 ) ) ;
#1633 = VERTEX_POINT ( 'NONE', #2696 ) ;
#1634 = ORIENTED_EDGE ( 'NONE', *, *, #12978, .F. ) ;
#1635 = DIRECTION ( 'NONE',  ( -2.797435172181481150E-17, 1.000000000000000000, -1.765856845898762549E-18 ) ) ;
#1636 = ORIENTED_EDGE ( 'NONE', *, *, #13462, .T. ) ;
#1637 = CARTESIAN_POINT ( 'NONE',  ( 4.216390066750006937, -117.2395442519084128, 3.627621796832325884 ) ) ;
#1638 = DIRECTION ( 'NONE',  ( -2.797435172181481150E-17, 1.000000000000000000, -1.765856845898762549E-18 ) ) ;
#1639 = EDGE_CURVE ( 'NONE', #5724, #13483, #3153, .T. ) ;
#1640 = DIRECTION ( 'NONE',  ( -1.000000000000000000, 0.000000000000000000, 0.000000000000000000 ) ) ;
#1641 = AXIS2_PLACEMENT_3D ( 'NONE', #4390, #8672, #12972 ) ;
#1642 = EDGE_CURVE ( 'NONE', #4432, #9210, #11254, .T. ) ;
#1643 = FACE_OUTER_BOUND ( 'NONE', #12202, .T. ) ;
#1644 = ORIENTED_EDGE ( 'NONE', *, *, #6867, .T. ) ;
#1645 = AXIS2_PLACEMENT_3D ( 'NONE', #6464, #9685, #92 ) ;
#1646 = ORIENTED_EDGE ( 'NONE', *, *, #2049, .T. ) ;
#1647 = CYLINDRICAL_SURFACE ( 'NONE', #7272, 5.999999999999998224 ) ;
#1648 = ADVANCED_FACE ( 'NONE', ( #9217 ), #8226, .T. ) ;
#1649 = CARTESIAN_POINT ( 'NONE',  ( 3.709034887389476509, -132.4786972693144662, -0.6210620215803320798 ) ) ;
#1650 = CARTESIAN_POINT ( 'NONE',  ( 4.330127018922190985, 91.86461561432780343, -2.500000000000000000 ) ) ;
#1651 = LINE ( 'NONE', #548, #1823 ) ;
#1652 = EDGE_CURVE ( 'NONE', #9058, #2729, #2495, .T. ) ;
#1653 = CARTESIAN_POINT ( 'NONE',  ( -6.999999999999999112, -20.00000000000000355, 7.500000000000000000 ) ) ;
#1654 = EDGE_CURVE ( 'NONE', #2621, #3550, #8315, .T. ) ;
#1655 = CARTESIAN_POINT ( 'NONE',  ( 15.29705854078139105, 19.67281349139174296, 1.840275709580740132E-15 ) ) ;
#1656 = CARTESIAN_POINT ( 'NONE',  ( 38.24615002434714484, 18.46584715143433542, 2.500000000000005329 ) ) ;
#1657 = CARTESIAN_POINT ( 'NONE',  ( -18.54049621773915746, 27.07720798311999388, -7.500000000000000000 ) ) ;
#1658 = CYLINDRICAL_SURFACE ( 'NONE', #316, 5.000000000000001776 ) ;
#1659 = VERTEX_POINT ( 'NONE', #7367 ) ;
#1660 = ORIENTED_EDGE ( 'NONE', *, *, #6019, .F. ) ;
#1661 = DIRECTION ( 'NONE',  ( 0.9960067511297464593, -0.08927794634716622324, 6.802837160686558945E-17 ) ) ;
#1662 = VERTEX_POINT ( 'NONE', #6326 ) ;
#1663 = EDGE_CURVE ( 'NONE', #3310, #9058, #3592, .T. ) ;
#1664 = ORIENTED_EDGE ( 'NONE', *, *, #3879, .F. ) ;
#1665 = CIRCLE ( 'NONE', #11719, 22.49999999999998934 ) ;
#1666 = DIRECTION ( 'NONE',  ( 0.000000000000000000, 0.000000000000000000, 1.000000000000000000 ) ) ;
#1667 = CARTESIAN_POINT ( 'NONE',  ( -35.00000000000000000, -4.286263797015736496E-15, 10.49999999999999822 ) ) ;
#1668 = CARTESIAN_POINT ( 'NONE',  ( -10.82118823930625418, -118.2727272727264420, -9.720764081409949853 ) ) ;
#1669 = EDGE_CURVE ( 'NONE', #1961, #973, #9882, .T. ) ;
#1670 = DIRECTION ( 'NONE',  ( -0.8907235428302473501, -0.4545454545454531425, -0.000000000000000000 ) ) ;
#1671 = CARTESIAN_POINT ( 'NONE',  ( -10.69381717166375623, -21.56444287793185666, -1.233455458826524398E-15 ) ) ;
#1672 = CARTESIAN_POINT ( 'NONE',  ( -15.18222645069203303, -16.04698886238941924, 4.000000000000000000 ) ) ;
#1673 = UNCERTAINTY_MEASURE_WITH_UNIT (LENGTH_MEASURE( 1.000000000000000082E-05 ), #11236, 'distance_accuracy_value', 'NONE');
#1674 = CARTESIAN_POINT ( 'NONE',  ( 9.115242562766566081, -73.26725376456661820, 4.373789808026823600 ) ) ;
#1675 = CIRCLE ( 'NONE', #2788, 8.385254915620292238 ) ;
#1676 = ORIENTED_EDGE ( 'NONE', *, *, #1120, .F. ) ;
#1677 = ORIENTED_EDGE ( 'NONE', *, *, #2791, .T. ) ;
#1678 = CARTESIAN_POINT ( 'NONE',  ( -1.210348956774063511, -80.16702553641545137, 10.05366391452042230 ) ) ;
#1679 = EDGE_LOOP ( 'NONE', ( #10985, #3054, #7344, #7916 ) ) ;
#1680 = CARTESIAN_POINT ( 'NONE',  ( 0.000000000000000000, 40.00000000000000000, 0.000000000000000000 ) ) ;
#1681 = CIRCLE ( 'NONE', #1227, 8.385254915620290461 ) ;
#1682 = DIRECTION ( 'NONE',  ( -1.000000000000000000, 0.000000000000000000, 0.000000000000000000 ) ) ;
#1683 = VECTOR ( 'NONE', #7325, 1000.000000000000000 ) ;
#1684 = CARTESIAN_POINT ( 'NONE',  ( 18.54049621773915746, 27.07720798312000809, -7.500000000000000000 ) ) ;
#1685 = CARTESIAN_POINT ( 'NONE',  ( -35.06230589874904524, 106.5835921350012825, 2.486789939184904430 ) ) ;
#1686 = CARTESIAN_POINT ( 'NONE',  ( 7.892147093659925616, -89.25378073177839156, -4.277061995178171649 ) ) ;
#1687 = FACE_OUTER_BOUND ( 'NONE', #8643, .T. ) ;
#1688 = EDGE_LOOP ( 'NONE', ( #13191, #9298, #10352, #13341 ) ) ;
#1689 = VECTOR ( 'NONE', #4035, 1000.000000000000000 ) ;
#1690 =( GEOMETRIC_REPRESENTATION_CONTEXT ( 3 ) GLOBAL_UNCERTAINTY_ASSIGNED_CONTEXT ( ( #1673 ) ) GLOBAL_UNIT_ASSIGNED_CONTEXT ( ( #11236, #12500, #12288 ) ) REPRESENTATION_CONTEXT ( 'NONE', 'WORKASPACE' ) );
#1691 = AXIS2_PLACEMENT_3D ( 'NONE', #9348, #794, #9415 ) ;
#1692 = CARTESIAN_POINT ( 'NONE',  ( 25.00000000000000355, 120.0000000000000284, -0.5000000000000000000 ) ) ;
#1693 = CARTESIAN_POINT ( 'NONE',  ( 6.726204760714201925, -75.54545454545360883, 7.481082188384250209 ) ) ;
#1694 = ORIENTED_EDGE ( 'NONE', *, *, #12378, .F. ) ;
#1695 = CARTESIAN_POINT ( 'NONE',  ( 2.255225228351934952, -77.73185732064989395, 9.851628683897507344 ) ) ;
#1696 =( NAMED_UNIT ( * ) PLANE_ANGLE_UNIT ( ) SI_UNIT ( $, .RADIAN. ) );
#1697 = DIRECTION ( 'NONE',  ( 0.01532218268402011502, -0.9998826084685129567, -2.891205793291787644E-16 ) ) ;
#1698 = CIRCLE ( 'NONE', #9311, 66.25000000000044054 ) ;
#1699 = CARTESIAN_POINT ( 'NONE',  ( 1.423465862495751466, -128.7272727272806492, -3.918423281948167691 ) ) ;
#1700 = CARTESIAN_POINT ( 'NONE',  ( 14.20591609908152009, -14.75994833063034761, 2.499999999999994671 ) ) ;
#1701 = CARTESIAN_POINT ( 'NONE',  ( 15.29705854078138749, 76.22148119144830503, 1.740418857596140842E-15 ) ) ;
#1702 = STYLED_ITEM ( 'NONE', ( #12834 ), #5722 ) ;
#1703 = CARTESIAN_POINT ( 'NONE',  ( 1.958204620527036497E-15, -70.00000000000000000, 1.236099792129133461E-16 ) ) ;
#1704 = CIRCLE ( 'NONE', #13621, 24.99999999999998934 ) ;
#1705 = VERTEX_POINT ( 'NONE', #7772 ) ;
#1706 = EDGE_CURVE ( 'NONE', #3550, #2621, #11671, .T. ) ;
#1707 = EDGE_LOOP ( 'NONE', ( #11988, #1976, #8800, #9233 ) ) ;
#1708 = FACE_OUTER_BOUND ( 'NONE', #10037, .T. ) ;
#1709 = ORIENTED_EDGE ( 'NONE', *, *, #11756, .F. ) ;
#1710 = CARTESIAN_POINT ( 'NONE',  ( -5.391851710260636921, -96.31036116225249089, -6.045474291746966600 ) ) ;
#1711 = AXIS2_PLACEMENT_3D ( 'NONE', #10520, #8355, #6123 ) ;
#1712 = DIRECTION ( 'NONE',  ( -2.797435172181481150E-17, 1.000000000000000000, -1.765856845898762549E-18 ) ) ;
#1713 = CARTESIAN_POINT ( 'NONE',  ( 35.08961652778860696, 18.74878582411816197, 2.500000000000005329 ) ) ;
#1714 = VERTEX_POINT ( 'NONE', #8912 ) ;
#1715 = DIRECTION ( 'NONE',  ( 0.000000000000000000, -1.000000000000000000, 0.000000000000000000 ) ) ;
#1716 = CARTESIAN_POINT ( 'NONE',  ( 0.1852016367012860043, -160.0000000000003126, -1.488522876466233713 ) ) ;
#1717 = CARTESIAN_POINT ( 'NONE',  ( 4.355466475183198247E-16, -15.56949922734665570, 2.749350679782564022E-17 ) ) ;
#1718 = DIRECTION ( 'NONE',  ( -2.797435172181481150E-17, 1.000000000000000000, -1.765856845898762549E-18 ) ) ;
#1719 = CARTESIAN_POINT ( 'NONE',  ( 17.19653809941365452, 5.878923826270381348, -2.499999999999999112 ) ) ;
#1720 = CYLINDRICAL_SURFACE ( 'NONE', #8580, 9.000000000008999024 ) ;
#1721 = VECTOR ( 'NONE', #11277, 1000.000000000000000 ) ;
#1722 = DIRECTION ( 'NONE',  ( 0.000000000000000000, 0.000000000000000000, 1.000000000000000000 ) ) ;
#1723 = FACE_OUTER_BOUND ( 'NONE', #3899, .T. ) ;
#1724 = EDGE_CURVE ( 'NONE', #7206, #13532, #6973, .T. ) ;
#1725 = ADVANCED_FACE ( 'NONE', ( #12062 ), #3294, .T. ) ;
#1726 = ORIENTED_EDGE ( 'NONE', *, *, #10712, .T. ) ;
#1727 = VERTEX_POINT ( 'NONE', #13780 ) ;
#1728 = DIRECTION ( 'NONE',  ( -6.158143864569485777E-17, -2.736152283717910599E-16, 1.000000000000000000 ) ) ;
#1729 = EDGE_CURVE ( 'NONE', #5794, #3209, #35, .T. ) ;
#1730 = EDGE_CURVE ( 'NONE', #13845, #5632, #4275, .T. ) ;
#1731 = EDGE_LOOP ( 'NONE', ( #2801, #8861, #13593, #2533 ) ) ;
#1732 = ORIENTED_EDGE ( 'NONE', *, *, #10569, .F. ) ;
#1733 = PLANE ( 'NONE',  #1445 ) ;
#1734 = CARTESIAN_POINT ( 'NONE',  ( 35.20000000000001705, 106.4000000000000199, -2.500000000000000000 ) ) ;
#1735 = CARTESIAN_POINT ( 'NONE',  ( -32.95454545454546746, 135.5876619995293311, -7.500000000000000000 ) ) ;
#1736 = CARTESIAN_POINT ( 'NONE',  ( 37.49001687782395464, -0.2231948658677927189, -47.50005079999998969 ) ) ;
#1737 = CARTESIAN_POINT ( 'NONE',  ( 34.66997162884352690, 21.14050806081579736, 2.500000000000005773 ) ) ;
#1738 = CARTESIAN_POINT ( 'NONE',  ( 12.99553232110413425, 20.49953269456136695, 25.99106464220827917 ) ) ;
#1739 = CARTESIAN_POINT ( 'NONE',  ( -4.330127018922195425, 92.00000000000000000, 2.500000000000000000 ) ) ;
#1740 = ORIENTED_EDGE ( 'NONE', *, *, #8641, .T. ) ;
#1741 = EDGE_CURVE ( 'NONE', #283, #13516, #1152, .T. ) ;
#1742 = EDGE_CURVE ( 'NONE', #10695, #7989, #11835, .T. ) ;
#1743 = CARTESIAN_POINT ( 'NONE',  ( -6.938012361950032236, -85.09891028704761595, 6.468549380687601769 ) ) ;
#1744 = B_SPLINE_CURVE_WITH_KNOTS ( 'NONE', 3,
 ( #11710, #3219, #13065, #1131, #13856, #6523, #2102, #11642, #5388, #11844, #10655, #2041, #10848, #2237, #9675, #8686 ),
 .UNSPECIFIED., .F., .F.,
 ( 4, 2, 2, 2, 2, 2, 2, 4 ),
 ( 0.001123485749927446119, 0.001530777205506870077, 0.001938068661086294036, 0.002345360116665717778, 0.002752651572245141953, 0.003159943027824565695, 0.003567234483403990304, 0.004381817394562847329 ),
 .UNSPECIFIED. ) ;
#1745 = VERTEX_POINT ( 'NONE', #13053 ) ;
#1746 = CARTESIAN_POINT ( 'NONE',  ( -37.50000000000000711, -4.286263797015736496E-15, 7.500000000000000000 ) ) ;
#1747 = DIRECTION ( 'NONE',  ( 0.000000000000000000, 0.000000000000000000, 1.000000000000000000 ) ) ;
#1748 = CARTESIAN_POINT ( 'NONE',  ( -1.815818965600183303E-15, 64.91013567203349055, -1.146220074446778111E-16 ) ) ;
#1749 = CARTESIAN_POINT ( 'NONE',  ( -4.752793807721118924, -119.4346283814399499, -2.305654517533438419 ) ) ;
#1750 = EDGE_CURVE ( 'NONE', #6075, #13845, #11971, .T. ) ;
#1751 = DIRECTION ( 'NONE',  ( -6.158143864569485777E-17, -2.736152283717910599E-16, 1.000000000000000000 ) ) ;
#1752 = AXIS2_PLACEMENT_3D ( 'NONE', #13, #7158, #2038 ) ;
#1753 = VERTEX_POINT ( 'NONE', #3704 ) ;
#1754 = ADVANCED_FACE ( 'NONE', ( #12267 ), #3629, .F. ) ;
#1755 = CYLINDRICAL_SURFACE ( 'NONE', #568, 2.500000000000002220 ) ;
#1756 = CIRCLE ( 'NONE', #9593, 25.50000000002549783 ) ;
#1757 = CARTESIAN_POINT ( 'NONE',  ( 10.03938689678732032, -69.87878787879145648, 0.2267434780641480463 ) ) ;
#1758 = ORIENTED_EDGE ( 'NONE', *, *, #8328, .T. ) ;
#1759 = CARTESIAN_POINT ( 'NONE',  ( 4.961404791891397714, 89.99999999999998579, 0.6346456166747422856 ) ) ;
#1760 = CIRCLE ( 'NONE', #10277, 66.25000000000044054 ) ;
#1761 = CARTESIAN_POINT ( 'NONE',  ( -25.00000000000000000, -35.00000000000000000, 7.500000000000000000 ) ) ;
#1762 = CARTESIAN_POINT ( 'NONE',  ( -8.355983821213438745, -73.45454545935436386, -17.50953411596619702 ) ) ;
#1763 = CARTESIAN_POINT ( 'NONE',  ( 26.79177319725820539, -26.24642857144861807, -4.000000000000000000 ) ) ;
#1764 = DIRECTION ( 'NONE',  ( -2.797435172181481150E-17, 1.000000000000000000, -1.765856845898762549E-18 ) ) ;
#1765 = CARTESIAN_POINT ( 'NONE',  ( 28.79177319725820183, -26.24642857144861807, 4.000000000000000000 ) ) ;
#1766 = ORIENTED_EDGE ( 'NONE', *, *, #8130, .F. ) ;
#1767 = ORIENTED_EDGE ( 'NONE', *, *, #13765, .T. ) ;
#1768 = CIRCLE ( 'NONE', #12538, 8.385254915620294014 ) ;
#1769 = ORIENTED_EDGE ( 'NONE', *, *, #10970, .T. ) ;
#1770 = DIRECTION ( 'NONE',  ( -6.158143864569485777E-17, -2.736152283717910599E-16, 1.000000000000000000 ) ) ;
#1771 = ORIENTED_EDGE ( 'NONE', *, *, #11775, .F. ) ;
#1772 = EDGE_CURVE ( 'NONE', #12816, #4304, #9219, .T. ) ;
#1773 = CARTESIAN_POINT ( 'NONE',  ( -34.99999999999999289, -97.00000000000000000, 7.500000000000000000 ) ) ;
#1774 = CARTESIAN_POINT ( 'NONE',  ( -35.00000000000000711, -25.00000000000000711, -4.000000000000000000 ) ) ;
#1775 = DIRECTION ( 'NONE',  ( -1.000000000000000000, 0.000000000000000000, 0.000000000000000000 ) ) ;
#1776 = CARTESIAN_POINT ( 'NONE',  ( 27.98552063842490867, -17.38741154648219833, -2.500000000000004441 ) ) ;
#1777 = CIRCLE ( 'NONE', #7363, 25.50000000002549783 ) ;
#1778 = DIRECTION ( 'NONE',  ( -1.224646799147353207E-16, 1.000000000000000000, -0.000000000000000000 ) ) ;
#1779 = DIRECTION ( 'NONE',  ( -2.797435172181481150E-17, 1.000000000000000000, -1.765856845898762549E-18 ) ) ;
#1780 = CARTESIAN_POINT ( 'NONE',  ( 12.99553232110414491, 1.649976794542512559, 1.591673766201862918E-15 ) ) ;
#1781 = AXIS2_PLACEMENT_3D ( 'NONE', #10677, #8646, #2395 ) ;
#1782 = CARTESIAN_POINT ( 'NONE',  ( -29.00000000000000355, -3.551475717527324818E-15, 8.499999999999998224 ) ) ;
#1783 = DIRECTION ( 'NONE',  ( 0.000000000000000000, 0.000000000000000000, 1.000000000000000000 ) ) ;
#1784 = B_SPLINE_CURVE_WITH_KNOTS ( 'NONE', 3,
 ( #5981, #1547, #2676, #4703 ),
 .UNSPECIFIED., .F., .F.,
 ( 4, 4 ),
 ( 0.02301878569831470461, 0.02656428146801016396 ),
 .UNSPECIFIED. ) ;
#1785 = ORIENTED_EDGE ( 'NONE', *, *, #556, .T. ) ;
#1786 = CARTESIAN_POINT ( 'NONE',  ( -35.20000000000000995, 106.3999999999999915, -2.500000000000000000 ) ) ;
#1787 = CARTESIAN_POINT ( 'NONE',  ( 36.36363636363638108, 142.2680885707561629, 0.5000000000000000000 ) ) ;
#1788 = AXIS2_PLACEMENT_3D ( 'NONE', #11891, #1242, #9791 ) ;
#1789 = ORIENTED_EDGE ( 'NONE', *, *, #1139, .F. ) ;
#1790 = CIRCLE ( 'NONE', #12787, 18.74900000001875000 ) ;
#1791 = ORIENTED_EDGE ( 'NONE', *, *, #7351, .T. ) ;
#1792 = DIRECTION ( 'NONE',  ( -2.797435172181481150E-17, 1.000000000000000000, -1.765856845898762549E-18 ) ) ;
#1793 = CARTESIAN_POINT ( 'NONE',  ( 10.69346802281034314, 59.02362407375952102, 0.000000000000000000 ) ) ;
#1794 = EDGE_CURVE ( 'NONE', #4611, #2641, #8895, .T. ) ;
#1795 = CARTESIAN_POINT ( 'NONE',  ( 3.469499284126810856, -73.45454542565497036, 20.14723442872987746 ) ) ;
#1796 = ADVANCED_FACE ( 'NONE', ( #6924 ), #8146, .T. ) ;
#1797 = CARTESIAN_POINT ( 'NONE',  ( -15.29705854078139282, 36.63580182200523438, -3.809726632991057923E-15 ) ) ;
#1798 = VECTOR ( 'NONE', #9395, 1000.000000000000000 ) ;
#1799 = CARTESIAN_POINT ( 'NONE',  ( 8.385254915620288685, 5.904668890677672088, 16.77050983124058448 ) ) ;
#1800 = DIRECTION ( 'NONE',  ( 0.000000000000000000, 0.000000000000000000, 1.000000000000000000 ) ) ;
#1801 = CIRCLE ( 'NONE', #484, 15.29705854078138749 ) ;
#1802 = LINE ( 'NONE', #6355, #10592 ) ;
#1803 = CIRCLE ( 'NONE', #12345, 9.000000000009002576 ) ;
#1804 = CARTESIAN_POINT ( 'NONE',  ( 18.44105126153190710, 8.793532718851094998, -2.499999999999998224 ) ) ;
#1805 = VERTEX_POINT ( 'NONE', #2434 ) ;
#1806 = VERTEX_POINT ( 'NONE', #11144 ) ;
#1807 = AXIS2_PLACEMENT_3D ( 'NONE', #12317, #10067, #2910 ) ;
#1808 = PRESENTATION_LAYER_ASSIGNMENT (  '', '', ( #2476 ) ) ;
#1809 = EDGE_CURVE ( 'NONE', #6479, #12375, #6718, .T. ) ;
#1810 = AXIS2_PLACEMENT_3D ( 'NONE', #8096, #7036, #6971 ) ;
#1811 = ORIENTED_EDGE ( 'NONE', *, *, #6765, .F. ) ;
#1812 = ORIENTED_EDGE ( 'NONE', *, *, #5748, .T. ) ;
#1813 = PLANE ( 'NONE',  #2040 ) ;
#1814 = EDGE_CURVE ( 'NONE', #2160, #10681, #6742, .T. ) ;
#1815 = CARTESIAN_POINT ( 'NONE',  ( 12.99553232110414491, 29.92431064457076673, -25.99106464220827561 ) ) ;
#1816 = EDGE_CURVE ( 'NONE', #7931, #7120, #9441, .T. ) ;
#1817 = CARTESIAN_POINT ( 'NONE',  ( -10.69346802281034670, 59.02362407375952102, -1.518026679872732817E-15 ) ) ;
#1818 = EDGE_CURVE ( 'NONE', #6908, #9709, #1234, .T. ) ;
#1819 = CARTESIAN_POINT ( 'NONE',  ( 35.66405164569891184, -18.73723662690267133, 2.499999999999994671 ) ) ;
#1820 = CARTESIAN_POINT ( 'NONE',  ( -0.009804802457270511001, -127.8804227454992457, -4.311392792372593874 ) ) ;
#1821 = DIRECTION ( 'NONE',  ( 0.1234677578012386701, 0.000000000000000000, -0.9923485843107424653 ) ) ;
#1822 =( BOUNDED_SURFACE ( )  B_SPLINE_SURFACE ( 3, 3, ( 
 ( #4284, #9559, #11790, #11524 ),
 ( #11593, #8435, #13868, #4215 ),
 ( #5137, #6465, #12793, #10667 ),
 ( #10729, #1148, #1982, #13669 ) ),
 .UNSPECIFIED., .F., .F., .T. ) 
 B_SPLINE_SURFACE_WITH_KNOTS ( ( 4, 4 ),
 ( 4, 4 ),
 ( 0.000000000000000000, 1.000000000000000000 ),
 ( 0.000000000000000000, 1.000000000000000000 ),
 .UNSPECIFIED. ) 
 GEOMETRIC_REPRESENTATION_ITEM ( )  RATIONAL_B_SPLINE_SURFACE ( (
 ( 1.000000000000000000, 0.3333333333333334259, 0.3333333333333334259, 1.000000000000000000),
 ( 1.000000000000000000, 0.3333333333333334259, 0.3333333333333334259, 1.000000000000000000),
 ( 1.000000000000000000, 0.3333333333333334259, 0.3333333333333334259, 1.000000000000000000),
 ( 1.000000000000000000, 0.3333333333333334259, 0.3333333333333334259, 1.000000000000000000) ) ) 
 REPRESENTATION_ITEM ( '' )  SURFACE ( )  );
#1823 = VECTOR ( 'NONE', #1850, 1000.000000000000000 ) ;
#1824 = AXIS2_PLACEMENT_3D ( 'NONE', #8707, #9911, #1280 ) ;
#1825 = ORIENTED_EDGE ( 'NONE', *, *, #6988, .T. ) ;
#1826 = ORIENTED_EDGE ( 'NONE', *, *, #375, .F. ) ;
#1827 = CARTESIAN_POINT ( 'NONE',  ( 43.29712336220986657, 19.44704974301885159, -2.499999999999993783 ) ) ;
#1828 = ORIENTED_EDGE ( 'NONE', *, *, #5654, .T. ) ;
#1829 = DIRECTION ( 'NONE',  ( -0.000000000000000000, -0.000000000000000000, -1.000000000000000000 ) ) ;
#1830 = EDGE_CURVE ( 'NONE', #2958, #4633, #7853, .T. ) ;
#1831 = ORIENTED_EDGE ( 'NONE', *, *, #6798, .T. ) ;
#1832 = CARTESIAN_POINT ( 'NONE',  ( -14.13596196814456718, -39.17949320881311337, -28.27192393628914502 ) ) ;
#1833 = VERTEX_POINT ( 'NONE', #13563 ) ;
#1834 = CARTESIAN_POINT ( 'NONE',  ( 12.99553232110413958, 11.07475474455194053, 0.000000000000000000 ) ) ;
#1835 = AXIS2_PLACEMENT_3D ( 'NONE', #3086, #5122, #7355 ) ;
#1836 = DIRECTION ( 'NONE',  ( 0.7999999999999996003, -0.6000000000000007550, 0.000000000000000000 ) ) ;
#1837 = CARTESIAN_POINT ( 'NONE',  ( -15.04986406078725203, -22.34153611474686940, 4.519294538364308167 ) ) ;
#1838 = ADVANCED_FACE ( 'NONE', ( #11285 ), #9653, .T. ) ;
#1839 = DIRECTION ( 'NONE',  ( -0.000000000000000000, -0.000000000000000000, -1.000000000000000000 ) ) ;
#1840 = CARTESIAN_POINT ( 'NONE',  ( -0.1372443476013192609, -156.3093790477994958, -1.553728524142399037 ) ) ;
#1841 = FACE_OUTER_BOUND ( 'NONE', #213, .T. ) ;
#1842 = ORIENTED_EDGE ( 'NONE', *, *, #11330, .T. ) ;
#1843 = ORIENTED_EDGE ( 'NONE', *, *, #5247, .T. ) ;
#1844 = CIRCLE ( 'NONE', #9670, 2.000000000000003997 ) ;
#1845 = DIRECTION ( 'NONE',  ( -6.158143864569485777E-17, -2.736152283717910599E-16, 1.000000000000000000 ) ) ;
#1846 = CARTESIAN_POINT ( 'NONE',  ( -15.29705854078138927, 38.52236939141059935, 30.59411708156276433 ) ) ;
#1847 = ORIENTED_EDGE ( 'NONE', *, *, #4187, .T. ) ;
#1848 = DIRECTION ( 'NONE',  ( -0.4226182617407014397, 0.9063077870366489375, 0.000000000000000000 ) ) ;
#1849 = CARTESIAN_POINT ( 'NONE',  ( -4.684139815134829021, -116.4556953340202909, -3.176431292803267414 ) ) ;
#1850 = DIRECTION ( 'NONE',  ( -0.000000000000000000, -0.000000000000000000, -1.000000000000000000 ) ) ;
#1851 = CYLINDRICAL_SURFACE ( 'NONE', #13242, 5.999999999999998224 ) ;
#1852 = DIRECTION ( 'NONE',  ( 1.000000000000000000, 0.000000000000000000, 0.000000000000000000 ) ) ;
#1853 = CARTESIAN_POINT ( 'NONE',  ( 39.06230589874905235, 109.5835921350012683, 2.499999999999999556 ) ) ;
#1854 = CARTESIAN_POINT ( 'NONE',  ( 15.29705854078138394, 29.09759144140119957, 30.59411708156277854 ) ) ;
#1855 = ADVANCED_FACE ( 'NONE', ( #11348 ), #10367, .F. ) ;
#1856 = DIRECTION ( 'NONE',  ( -0.000000000000000000, -0.000000000000000000, -1.000000000000000000 ) ) ;
#1857 = ORIENTED_EDGE ( 'NONE', *, *, #573, .T. ) ;
#1858 = AXIS2_PLACEMENT_3D ( 'NONE', #13495, #6022, #2582 ) ;
#1859 = CARTESIAN_POINT ( 'NONE',  ( 22.49448184590488609, 22.22300645049885048, 2.500000000000005329 ) ) ;
#1860 = ORIENTED_EDGE ( 'NONE', *, *, #3852, .T. ) ;
#1861 = CARTESIAN_POINT ( 'NONE',  ( 25.00000000000000355, 120.0000000000000142, 0.5000000000000000000 ) ) ;
#1862 = CIRCLE ( 'NONE', #4780, 1.999999999999998224 ) ;
#1863 = ORIENTED_EDGE ( 'NONE', *, *, #8017, .T. ) ;
#1864 = CARTESIAN_POINT ( 'NONE',  ( -8.385254915620295790, -12.94488700934118341, 16.77050983124058448 ) ) ;
#1865 = EDGE_LOOP ( 'NONE', ( #7834, #6382, #7851, #1377 ) ) ;
#1866 = DIRECTION ( 'NONE',  ( -0.000000000000000000, -0.000000000000000000, -1.000000000000000000 ) ) ;
#1867 = AXIS2_PLACEMENT_3D ( 'NONE', #4523, #9939, #6567 ) ;
#1868 = CARTESIAN_POINT ( 'NONE',  ( -15.48128881649354405, -16.40999965198128052, 2.699219240941213460 ) ) ;
#1869 = LINE ( 'NONE', #12679, #11839 ) ;
#1870 = AXIS2_PLACEMENT_3D ( 'NONE', #3571, #12221, #11235 ) ;
#1871 = CARTESIAN_POINT ( 'NONE',  ( 3.606245374316391583, -157.8181818183015821, -2.267989313183790934 ) ) ;
#1872 = VECTOR ( 'NONE', #5601, 1000.000000000000000 ) ;
#1873 = DIRECTION ( 'NONE',  ( -1.000000000000000000, 0.000000000000000000, 0.000000000000000000 ) ) ;
#1874 = CARTESIAN_POINT ( 'NONE',  ( 10.00000000000000000, 92.00000000000000000, 2.500000000000000000 ) ) ;
#1875 = CARTESIAN_POINT ( 'NONE',  ( -10.00000000000000711, 139.9999999999999716, 2.500000000000000000 ) ) ;
#1876 = CARTESIAN_POINT ( 'NONE',  ( -4.942648287111191863, 90.01344868170882307, 0.7664870281642331973 ) ) ;
#1877 = AXIS2_PLACEMENT_3D ( 'NONE', #2612, #4708, #3983 ) ;
#1878 = ORIENTED_EDGE ( 'NONE', *, *, #90, .F. ) ;
#1879 =( BOUNDED_SURFACE ( )  B_SPLINE_SURFACE ( 3, 3, ( 
 ( #5558, #326, #9711, #4582 ),
 ( #10883, #3255, #10684, #7529 ),
 ( #12019, #1293, #4509, #7466 ),
 ( #7735, #11810, #13100, #8867 ) ),
 .UNSPECIFIED., .F., .F., .T. ) 
 B_SPLINE_SURFACE_WITH_KNOTS ( ( 4, 4 ),
 ( 4, 4 ),
 ( 0.000000000000000000, 1.000000000000000000 ),
 ( 0.000000000000000000, 1.000000000000000000 ),
 .UNSPECIFIED. ) 
 GEOMETRIC_REPRESENTATION_ITEM ( )  RATIONAL_B_SPLINE_SURFACE ( (
 ( 1.000000000000000000, 0.3333333333333334259, 0.3333333333333334259, 1.000000000000000000),
 ( 1.000000000000000000, 0.3333333333333334259, 0.3333333333333334259, 1.000000000000000000),
 ( 1.000000000000000000, 0.3333333333333334259, 0.3333333333333334259, 1.000000000000000000),
 ( 1.000000000000000000, 0.3333333333333334259, 0.3333333333333334259, 1.000000000000000000) ) ) 
 REPRESENTATION_ITEM ( '' )  SURFACE ( )  );
#1880 = CARTESIAN_POINT ( 'NONE',  ( -6.798205150802573371, -84.93498744380758581, 6.637038377984636917 ) ) ;
#1881 = DIRECTION ( 'NONE',  ( -1.224646799147353207E-16, 1.000000000000000000, -0.000000000000000000 ) ) ;
#1882 = CARTESIAN_POINT ( 'NONE',  ( -24.99999999999998934, -99.15310334213020838, 4.530792947966844994E-20 ) ) ;
#1883 = DIRECTION ( 'NONE',  ( -0.000000000000000000, -0.000000000000000000, -1.000000000000000000 ) ) ;
#1884 = TOROIDAL_SURFACE ( 'NONE', #8383, 77.49999999999998579, 5.000000000000000000 ) ;
#1885 = FACE_OUTER_BOUND ( 'NONE', #3585, .T. ) ;
#1886 = CARTESIAN_POINT ( 'NONE',  ( 2.435310979999304237, -143.3834574191564002, 0.8240421561592208288 ) ) ;
#1887 = DIRECTION ( 'NONE',  ( -0.8000000000000008216, 0.5999999999999988676, 0.000000000000000000 ) ) ;
#1888 = ORIENTED_EDGE ( 'NONE', *, *, #448, .T. ) ;
#1889 = EDGE_CURVE ( 'NONE', #12845, #7874, #12943, .T. ) ;
#1890 = VERTEX_POINT ( 'NONE', #462 ) ;
#1891 = EDGE_CURVE ( 'NONE', #3176, #9535, #2765, .T. ) ;
#1892 = ORIENTED_EDGE ( 'NONE', *, *, #8431, .T. ) ;
#1893 = EDGE_CURVE ( 'NONE', #13392, #7522, #6891, .T. ) ;
#1894 = CIRCLE ( 'NONE', #9727, 8.385254915620295790 ) ;
#1895 = EDGE_CURVE ( 'NONE', #5016, #8361, #13461, .T. ) ;
#1896 = CIRCLE ( 'NONE', #5250, 14.99999999999998934 ) ;
#1897 = EDGE_CURVE ( 'NONE', #3490, #7522, #2043, .T. ) ;
#1898 = ORIENTED_EDGE ( 'NONE', *, *, #3506, .T. ) ;
#1899 = CARTESIAN_POINT ( 'NONE',  ( 35.00000000000000000, 4.286263797015736496E-15, 7.500000000000000000 ) ) ;
#1900 = ORIENTED_EDGE ( 'NONE', *, *, #7122, .F. ) ;
#1901 = ORIENTED_EDGE ( 'NONE', *, *, #2761, .F. ) ;
#1902 = DIRECTION ( 'NONE',  ( -6.158143864569485777E-17, -2.736152283717910599E-16, 1.000000000000000000 ) ) ;
#1903 = CARTESIAN_POINT ( 'NONE',  ( -9.846850911399156914, -91.60173160168641004, 0.3733502116265231541 ) ) ;
#1904 = CARTESIAN_POINT ( 'NONE',  ( -8.385254915620292238, 43.60378069071538221, 16.77050983124057382 ) ) ;
#1905 =( BOUNDED_SURFACE ( )  B_SPLINE_SURFACE ( 3, 3, ( 
 ( #3089, #10521, #5195, #13790 ),
 ( #6319, #996, #9549, #12781 ),
 ( #10656, #9611, #16, #12854 ),
 ( #3220, #6802, #10781, #2301 ) ),
 .UNSPECIFIED., .F., .F., .T. ) 
 B_SPLINE_SURFACE_WITH_KNOTS ( ( 4, 4 ),
 ( 4, 4 ),
 ( 0.000000000000000000, 1.000000000000000000 ),
 ( 0.000000000000000000, 1.000000000000000000 ),
 .UNSPECIFIED. ) 
 GEOMETRIC_REPRESENTATION_ITEM ( )  RATIONAL_B_SPLINE_SURFACE ( (
 ( 1.000000000000000000, 0.3333333333333334259, 0.3333333333333334259, 1.000000000000000000),
 ( 1.000000000000000000, 0.3333333333333334259, 0.3333333333333334259, 1.000000000000000000),
 ( 1.000000000000000000, 0.3333333333333334259, 0.3333333333333334259, 1.000000000000000000),
 ( 1.000000000000000000, 0.3333333333333334259, 0.3333333333333334259, 1.000000000000000000) ) ) 
 REPRESENTATION_ITEM ( '' )  SURFACE ( )  );
#1906 = CARTESIAN_POINT ( 'NONE',  ( 34.99999999999958789, 1.104930248025249758E-13, -2.499999999999999112 ) ) ;
#1907 = CARTESIAN_POINT ( 'NONE',  ( 2.678949786664373445, -123.4179834144425740, 4.050618884325445812 ) ) ;
#1908 = CARTESIAN_POINT ( 'NONE',  ( 35.20000000000002416, 106.3999999999999915, 0.5000000000000000000 ) ) ;
#1909 = CIRCLE ( 'NONE', #11972, 48.00000000000001421 ) ;
#1910 = ORIENTED_EDGE ( 'NONE', *, *, #9040, .T. ) ;
#1911 = ORIENTED_EDGE ( 'NONE', *, *, #6137, .T. ) ;
#1912 = AXIS2_PLACEMENT_3D ( 'NONE', #6617, #9993, #3453 ) ;
#1913 = VERTEX_POINT ( 'NONE', #12437 ) ;
#1914 = EDGE_CURVE ( 'NONE', #8462, #8344, #10106, .T. ) ;
#1915 = CARTESIAN_POINT ( 'NONE',  ( 55.20422767451771051, -6.230504303137472277, 2.499999999999999556 ) ) ;
#1916 = CIRCLE ( 'NONE', #9977, 25.50000000002550138 ) ;
#1917 = DIRECTION ( 'NONE',  ( -0.000000000000000000, -0.000000000000000000, -1.000000000000000000 ) ) ;
#1918 = CARTESIAN_POINT ( 'NONE',  ( 3.127593042865025375, -81.56118865055866252, -9.358713454693210920 ) ) ;
#1919 = CARTESIAN_POINT ( 'NONE',  ( 0.3237100442286745539, -158.0606060622567668, 0.5247744424694577026 ) ) ;
#1920 = CARTESIAN_POINT ( 'NONE',  ( 39.06230589874904524, 109.5835921350012683, 2.499999999999999556 ) ) ;
#1921 = DIRECTION ( 'NONE',  ( -1.000000000000000000, 0.000000000000000000, 0.000000000000000000 ) ) ;
#1922 = CIRCLE ( 'NONE', #6395, 66.25000000000044054 ) ;
#1923 = CYLINDRICAL_SURFACE ( 'NONE', #1038, 8.385254915620292238 ) ;
#1924 = CYLINDRICAL_SURFACE ( 'NONE', #7839, 15.29705854078139105 ) ;
#1925 = CARTESIAN_POINT ( 'NONE',  ( 25.00000000000001776, -99.52837026979787538, -3.391106264173641804 ) ) ;
#1926 = CARTESIAN_POINT ( 'NONE',  ( -35.00000000000000000, -4.286263797015736496E-15, -4.000000000000000000 ) ) ;
#1927 = CIRCLE ( 'NONE', #6627, 5.000000000000000000 ) ;
#1928 = DIRECTION ( 'NONE',  ( -0.4545454545454558626, 0.8907235428302457958, 0.000000000000000000 ) ) ;
#1929 = VERTEX_POINT ( 'NONE', #9140 ) ;
#1930 = DIRECTION ( 'NONE',  ( -2.797435172181481150E-17, 1.000000000000000000, -1.765856845898762549E-18 ) ) ;
#1931 = CYLINDRICAL_SURFACE ( 'NONE', #12325, 20.00000000000000000 ) ;
#1932 = CARTESIAN_POINT ( 'NONE',  ( 2.710744138662893210, -134.9675367765264582, -2.173820228074841321 ) ) ;
#1933 = CARTESIAN_POINT ( 'NONE',  ( -3.867425345466811493, -111.7272727272759454, 3.383301718857328666 ) ) ;
#1934 = AXIS2_PLACEMENT_3D ( 'NONE', #9679, #7434, #6389 ) ;
#1935 = ADVANCED_FACE ( 'NONE', ( #1708 ), #11103, .F. ) ;
#1936 = ORIENTED_EDGE ( 'NONE', *, *, #5084, .F. ) ;
#1937 = CARTESIAN_POINT ( 'NONE',  ( -35.06230589874904524, 106.5835921350012825, 2.486789939184904430 ) ) ;
#1938 = ORIENTED_EDGE ( 'NONE', *, *, #6260, .F. ) ;
#1939 = DIRECTION ( 'NONE',  ( -0.000000000000000000, -0.000000000000000000, 1.000000000000000000 ) ) ;
#1940 = DIRECTION ( 'NONE',  ( -6.158143864569485777E-17, -2.736152283717910599E-16, 1.000000000000000000 ) ) ;
#1941 = CARTESIAN_POINT ( 'NONE',  ( 8.012933684613601670, -76.12121211522740793, 3.597289648239124116 ) ) ;
#1942 = CARTESIAN_POINT ( 'NONE',  ( 2.503528417663046124, -105.1818181818193096, -12.81920766435407089 ) ) ;
#1943 = CARTESIAN_POINT ( 'NONE',  ( -8.385254915620299343, 50.40394642271930081, 16.77050983124058803 ) ) ;
#1944 = DIRECTION ( 'NONE',  ( -0.5999999999999966471, 0.8000000000000024869, 0.000000000000000000 ) ) ;
#1945 = CARTESIAN_POINT ( 'NONE',  ( 155.9864723944028810, -111.6214737678657087, 2.500000000000000000 ) ) ;
#1946 = VECTOR ( 'NONE', #3403, 1000.000000000000000 ) ;
#1947 = VERTEX_POINT ( 'NONE', #13237 ) ;
#1948 = EDGE_CURVE ( 'NONE', #2799, #11270, #12812, .T. ) ;
#1949 = ORIENTED_EDGE ( 'NONE', *, *, #816, .F. ) ;
#1950 = CARTESIAN_POINT ( 'NONE',  ( 12.99579180576517778, -20.73949187309215247, -25.99158361153034136 ) ) ;
#1951 = CARTESIAN_POINT ( 'NONE',  ( -34.99999999999999289, -97.00000000000000000, 7.500000000000000000 ) ) ;
#1952 = EDGE_CURVE ( 'NONE', #849, #717, #5857, .T. ) ;
#1953 = DIRECTION ( 'NONE',  ( -1.000000000000000000, 0.000000000000000000, 0.000000000000000000 ) ) ;
#1954 = DIRECTION ( 'NONE',  ( 0.000000000000000000, -1.000000000000000000, 0.000000000000000000 ) ) ;
#1955 = CARTESIAN_POINT ( 'NONE',  ( 0.3217016761801410052, -154.7285720644513844, 1.606987287732108527 ) ) ;
#1956 = CARTESIAN_POINT ( 'NONE',  ( 12.99553232110413958, 48.77386654458962312, 1.520979731354686344E-15 ) ) ;
#1957 = ORIENTED_EDGE ( 'NONE', *, *, #5433, .T. ) ;
#1958 = ORIENTED_EDGE ( 'NONE', *, *, #3431, .T. ) ;
#1959 = EDGE_LOOP ( 'NONE', ( #2546, #8274, #1644, #8029 ) ) ;
#1960 = DIRECTION ( 'NONE',  ( -1.000000000000000000, -1.224646799147353207E-16, 0.000000000000000000 ) ) ;
#1961 = VERTEX_POINT ( 'NONE', #13311 ) ;
#1962 = ORIENTED_EDGE ( 'NONE', *, *, #10232, .F. ) ;
#1963 = CARTESIAN_POINT ( 'NONE',  ( 8.385254915620294014, 78.67828027274755698, 9.540301975042864801E-16 ) ) ;
#1964 = EDGE_LOOP ( 'NONE', ( #10298, #4928, #5699, #8290 ) ) ;
#1965 = DIRECTION ( 'NONE',  ( 0.9960067511297463483, -0.08927794634716618161, 4.818676322152979407E-17 ) ) ;
#1966 = EDGE_CURVE ( 'NONE', #4027, #1473, #4698, .T. ) ;
#1967 = CARTESIAN_POINT ( 'NONE',  ( 32.72727272727274084, 135.1423002281142089, 0.5000000000000000000 ) ) ;
#1968 = EDGE_CURVE ( 'NONE', #6184, #2827, #6710, .T. ) ;
#1969 = CARTESIAN_POINT ( 'NONE',  ( 25.00000000000001421, -34.99999999999999289, 7.500000000000000000 ) ) ;
#1970 = CARTESIAN_POINT ( 'NONE',  ( -10.82460162405759263, -71.99999999999995737, -2.658570984655005631 ) ) ;
#1971 = DIRECTION ( 'NONE',  ( -1.000000000000000000, 0.000000000000000000, 0.000000000000000000 ) ) ;
#1972 = FACE_OUTER_BOUND ( 'NONE', #6824, .T. ) ;
#1973 = CARTESIAN_POINT ( 'NONE',  ( -1.819570364555604502, -146.4201944892890879, -1.378504945579682062 ) ) ;
#1974 = EDGE_CURVE ( 'NONE', #887, #3550, #3586, .T. ) ;
#1975 = FACE_OUTER_BOUND ( 'NONE', #9275, .T. ) ;
#1976 = ORIENTED_EDGE ( 'NONE', *, *, #2575, .T. ) ;
#1977 = VERTEX_POINT ( 'NONE', #12789 ) ;
#1978 = ORIENTED_EDGE ( 'NONE', *, *, #11261, .F. ) ;
#1979 = CIRCLE ( 'NONE', #3770, 9.000000000009002576 ) ;
#1980 = CIRCLE ( 'NONE', #6906, 8.385254915620294014 ) ;
#1981 = DIRECTION ( 'NONE',  ( -6.158143864569485777E-17, -2.736152283717910599E-16, 1.000000000000000000 ) ) ;
#1982 = CARTESIAN_POINT ( 'NONE',  ( -15.29705854078138216, 38.52236939141059935, -30.59411708156276788 ) ) ;
#1983 = CARTESIAN_POINT ( 'NONE',  ( -5.313449998973543309, -115.2025049533512799, -2.323891416253867082 ) ) ;
#1984 = EDGE_CURVE ( 'NONE', #4263, #6792, #13709, .T. ) ;
#1985 = CARTESIAN_POINT ( 'NONE',  ( -0.7701066202684672124, -168.0000000000000568, -1.909695209560596796 ) ) ;
#1986 = FACE_OUTER_BOUND ( 'NONE', #12322, .T. ) ;
#1987 = EDGE_CURVE ( 'NONE', #10906, #7855, #6496, .T. ) ;
#1988 = DIRECTION ( 'NONE',  ( -0.000000000000000000, -0.000000000000000000, -1.000000000000000000 ) ) ;
#1989 = CARTESIAN_POINT ( 'NONE',  ( -12.99553232110413781, 1.649976794542511671, -25.99106464220828627 ) ) ;
#1990 = VECTOR ( 'NONE', #3207, 1000.000000000000000 ) ;
#1991 = DIRECTION ( 'NONE',  ( 0.9960067511297464593, -0.08927794634716622324, 3.401418580343279473E-17 ) ) ;
#1992 = ADVANCED_FACE ( 'NONE', ( #5131, #8295 ), #4146, .F. ) ;
#1993 = CARTESIAN_POINT ( 'NONE',  ( -8.385254915620294014, 59.82872437272870769, -1.056489625149731375E-16 ) ) ;
#1994 = EDGE_CURVE ( 'NONE', #13048, #8282, #10954, .T. ) ;
#1995 = CARTESIAN_POINT ( 'NONE',  ( 11.81226048336477064, -40.00941361824963849, 0.000000000000000000 ) ) ;
#1996 = CARTESIAN_POINT ( 'NONE',  ( -15.29705854078139282, 90.00000000000000000, -1.589271161308885878E-16 ) ) ;
#1997 = DIRECTION ( 'NONE',  ( 0.000000000000000000, 0.000000000000000000, 1.000000000000000000 ) ) ;
#1998 = CARTESIAN_POINT ( 'NONE',  ( -0.01432886326384079194, -82.89610389603521412, -5.147384767215601009 ) ) ;
#1999 = EDGE_LOOP ( 'NONE', ( #12155, #9038, #1616, #5906 ) ) ;
#2000 = FACE_OUTER_BOUND ( 'NONE', #12656, .T. ) ;
#2001 = AXIS2_PLACEMENT_3D ( 'NONE', #7506, #28, #9822 ) ;
#2002 = ORIENTED_EDGE ( 'NONE', *, *, #12623, .T. ) ;
#2003 = LINE ( 'NONE', #6284, #3458 ) ;
#2004 = CARTESIAN_POINT ( 'NONE',  ( 32.50000000000000000, 4.286263797015736496E-15, 4.000000000000000000 ) ) ;
#2005 = CLOSED_SHELL ( 'NONE', ( #4581, #9687, #11319, #9460, #3588, #10218, #432, #8396, #12006, #5588, #1563, #10694, #6032, #9638, #13585, #7458, #2471, #10229, #10027, #9796, #11511, #11935, #7208, #3950, #13273, #1123, #134, #12776, #635, #4031, #7282, #4048, #1855, #1935, #7213, #1142, #11590, #373, #8410, #7642, #10385, #2232, #9948, #11328, #12394, #6267, #11141, #2908, #12565, #9946, #4471, #7700, #5610, #12266, #276, #9178, #10300, #11770, #8830, #5086, #5399, #3266, #9691, #8262 ) ) ;
#2006 = CARTESIAN_POINT ( 'NONE',  ( 15.70089697932620609, -22.78139155752743861, -0.6412871628180832895 ) ) ;
#2007 = ADVANCED_FACE ( 'NONE', ( #10967 ), #8662, .F. ) ;
#2008 = CARTESIAN_POINT ( 'NONE',  ( -4.560784247219692666, -95.36363636362557372, -0.7586904865638435247 ) ) ;
#2009 = EDGE_CURVE ( 'NONE', #9777, #13779, #6942, .T. ) ;
#2010 = CARTESIAN_POINT ( 'NONE',  ( -2.517691654963332357E-15, 90.00000000000000000, -1.589271161308885878E-16 ) ) ;
#2011 = CARTESIAN_POINT ( 'NONE',  ( -4.769534092270762748, 90.26591089801031842, 1.504791211541889329 ) ) ;
#2012 = VECTOR ( 'NONE', #7587, 1000.000000000000000 ) ;
#2013 = ORIENTED_EDGE ( 'NONE', *, *, #7115, .T. ) ;
#2014 = AXIS2_PLACEMENT_3D ( 'NONE', #9048, #7925, #2598 ) ;
#2015 = EDGE_LOOP ( 'NONE', ( #12881, #12979, #6300, #7435 ) ) ;
#2016 = CARTESIAN_POINT ( 'NONE',  ( -15.29705854078139282, -10.48808792804187284, -3.755586217998579266E-15 ) ) ;
#2017 = CARTESIAN_POINT ( 'NONE',  ( 39.99999999999999289, 120.0000000000000142, 0.5000000000000000000 ) ) ;
#2018 = CIRCLE ( 'NONE', #9858, 2.000000000000000000 ) ;
#2019 = AXIS2_PLACEMENT_3D ( 'NONE', #8212, #2034, #9263 ) ;
#2020 = CARTESIAN_POINT ( 'NONE',  ( 15.29705854078138927, 29.09759144140119957, 1.823632900916640480E-15 ) ) ;
#2021 = CARTESIAN_POINT ( 'NONE',  ( -8.385254915620292238, -3.520109059331755663, -2.049896454535566708E-15 ) ) ;
#2022 = DIRECTION ( 'NONE',  ( -1.000000000000000000, 0.000000000000000000, 0.000000000000000000 ) ) ;
#2023 = DIRECTION ( 'NONE',  ( 1.000000000000000000, 0.000000000000000000, 0.000000000000000000 ) ) ;
#2024 = ORIENTED_EDGE ( 'NONE', *, *, #5099, .T. ) ;
#2025 = VERTEX_POINT ( 'NONE', #7606 ) ;
#2026 = ORIENTED_EDGE ( 'NONE', *, *, #970, .F. ) ;
#2027 = DIRECTION ( 'NONE',  ( -0.000000000000000000, -0.000000000000000000, -1.000000000000000000 ) ) ;
#2028 = AXIS2_PLACEMENT_3D ( 'NONE', #1362, #5641, #7963 ) ;
#2029 = AXIS2_PLACEMENT_3D ( 'NONE', #1827, #848, #9470 ) ;
#2030 = ORIENTED_EDGE ( 'NONE', *, *, #10110, .T. ) ;
#2031 = CARTESIAN_POINT ( 'NONE',  ( -2.771542151761396955, 90.01585036846415733, -4.174539845741943367 ) ) ;
#2032 = VERTEX_POINT ( 'NONE', #6631 ) ;
#2033 = ORIENTED_EDGE ( 'NONE', *, *, #1219, .T. ) ;
#2034 = DIRECTION ( 'NONE',  ( -0.5952233065713573579, -0.8035603370713738647, -3.056366244416775696E-15 ) ) ;
#2035 = ORIENTED_EDGE ( 'NONE', *, *, #400, .F. ) ;
#2036 = CARTESIAN_POINT ( 'NONE',  ( -35.00000000000000000, -4.286263797015736496E-15, 7.500000000000000000 ) ) ;
#2037 = TOROIDAL_SURFACE ( 'NONE', #5612, 22.99999999999999289, 2.000000000000000000 ) ;
#2038 = DIRECTION ( 'NONE',  ( 0.9960067511297464593, -0.08927794634716622324, 3.401418580343279473E-17 ) ) ;
#2039 = CARTESIAN_POINT ( 'NONE',  ( -9.412634226148453465, -72.00000000000004263, -5.970118669234189213 ) ) ;
#2040 = AXIS2_PLACEMENT_3D ( 'NONE', #8201, #4116, #12482 ) ;
#2041 = CARTESIAN_POINT ( 'NONE',  ( 40.49366238756158509, 100.7360090884195216, -1.526167340029800146 ) ) ;
#2042 = CARTESIAN_POINT ( 'NONE',  ( 0.000000000000000000, -20.00000000000000355, 0.000000000000000000 ) ) ;
#2043 = CIRCLE ( 'NONE', #13515, 2.500000000000002220 ) ;
#2044 = CARTESIAN_POINT ( 'NONE',  ( -0.6071592415733604309, -152.6372033014571343, -1.642897721265916822 ) ) ;
#2045 = DIRECTION ( 'NONE',  ( 1.000000000000000000, 0.000000000000000000, 0.000000000000000000 ) ) ;
#2046 = EDGE_LOOP ( 'NONE', ( #2111, #2784, #3306, #10881 ) ) ;
#2047 = ORIENTED_EDGE ( 'NONE', *, *, #9173, .T. ) ;
#2048 = VERTEX_POINT ( 'NONE', #4517 ) ;
#2049 = EDGE_CURVE ( 'NONE', #11046, #11768, #7829, .T. ) ;
#2050 = CARTESIAN_POINT ( 'NONE',  ( -0.5594493140154206401, -142.1330619314459796, -2.638491898088323850 ) ) ;
#2051 = VECTOR ( 'NONE', #7783, 1000.000000000000000 ) ;
#2052 = ORIENTED_EDGE ( 'NONE', *, *, #10986, .T. ) ;
#2053 = DIRECTION ( 'NONE',  ( -2.797435172181481150E-17, 1.000000000000000000, -1.765856845898762549E-18 ) ) ;
#2054 = CARTESIAN_POINT ( 'NONE',  ( -3.914066993105319359, -117.7082033709801578, -3.866271586310865871 ) ) ;
#2055 = DIRECTION ( 'NONE',  ( 1.000000000000000000, 0.000000000000000000, 0.000000000000000000 ) ) ;
#2056 = DIRECTION ( 'NONE',  ( 1.000000000000000000, 0.000000000000000000, 0.000000000000000000 ) ) ;
#2057 = CARTESIAN_POINT ( 'NONE',  ( 35.06230589874905945, 106.5835921350012683, 7.500000000000000000 ) ) ;
#2058 = DIRECTION ( 'NONE',  ( -2.797435172181481150E-17, 1.000000000000000000, -1.765856845898762549E-18 ) ) ;
#2059 = DIRECTION ( 'NONE',  ( -0.000000000000000000, -0.000000000000000000, -1.000000000000000000 ) ) ;
#2060 = CIRCLE ( 'NONE', #9898, 2.000000000000007105 ) ;
#2061 = CARTESIAN_POINT ( 'NONE',  ( 35.06230589874905945, 106.5835921350012683, 7.500000000000000000 ) ) ;
#2062 = EDGE_CURVE ( 'NONE', #1545, #10464, #6058, .T. ) ;
#2063 = B_SPLINE_CURVE_WITH_KNOTS ( 'NONE', 3,
 ( #8757, #9610, #10590, #12780, #3151, #7357, #1195, #4201 ),
 .UNSPECIFIED., .F., .F.,
 ( 4, 2, 2, 4 ),
 ( 0.02696056912299139158, 0.02949568642151887896, 0.03076324507078262438, 0.03203080372004636633 ),
 .UNSPECIFIED. ) ;
#2064 = DIRECTION ( 'NONE',  ( -1.150550675996984260E-16, -1.357138225298697177E-16, 1.000000000000000000 ) ) ;
#2065 = EDGE_CURVE ( 'NONE', #10096, #2984, #905, .T. ) ;
#2066 = EDGE_LOOP ( 'NONE', ( #6390, #569, #4598, #7412, #5148 ) ) ;
#2067 = FACE_OUTER_BOUND ( 'NONE', #13413, .T. ) ;
#2068 = ADVANCED_FACE ( 'NONE', ( #337 ), #4594, .T. ) ;
#2069 = ORIENTED_EDGE ( 'NONE', *, *, #6685, .F. ) ;
#2070 = CARTESIAN_POINT ( 'NONE',  ( -25.00000000000000355, 120.0000000000000142, 2.500000000000000000 ) ) ;
#2071 = EDGE_CURVE ( 'NONE', #4214, #5708, #9630, .T. ) ;
#2072 = DIRECTION ( 'NONE',  ( 0.000000000000000000, 1.000000000000000000, -0.000000000000000000 ) ) ;
#2073 = DIRECTION ( 'NONE',  ( -2.797435172181481150E-17, 1.000000000000000000, -1.765856845898762549E-18 ) ) ;
#2074 = CARTESIAN_POINT ( 'NONE',  ( 2.518175769240307726, -124.8181818181797240, 12.81633841918553607 ) ) ;
#2075 = CARTESIAN_POINT ( 'NONE',  ( -41.00000000000000000, -4.286263797015736496E-15, 10.49999999999999822 ) ) ;
#2076 = DIRECTION ( 'NONE',  ( 0.8000000000000000444, -0.5999999999999999778, 0.000000000000000000 ) ) ;
#2077 = DIRECTION ( 'NONE',  ( -1.000000000000000000, 0.000000000000000000, 0.000000000000000000 ) ) ;
#2078 = DIRECTION ( 'NONE',  ( -2.797435172181481150E-17, 1.000000000000000000, -1.765856845898762549E-18 ) ) ;
#2079 = DIRECTION ( 'NONE',  ( -2.797435172181479917E-17, 1.000000000000000000, -1.765856845898779112E-18 ) ) ;
#2080 = VECTOR ( 'NONE', #10962, 1000.000000000000000 ) ;
#2081 = ORIENTED_EDGE ( 'NONE', *, *, #13499, .T. ) ;
#2082 = EDGE_CURVE ( 'NONE', #6129, #4849, #10611, .T. ) ;
#2083 = VERTEX_POINT ( 'NONE', #6275 ) ;
#2084 = CARTESIAN_POINT ( 'NONE',  ( -8.385254915620292238, 43.60378069071538221, -2.162292655033656152E-15 ) ) ;
#2085 = LINE ( 'NONE', #11621, #5695 ) ;
#2086 = CARTESIAN_POINT ( 'NONE',  ( -12.99553232110413425, 29.92431064457076673, -25.99106464220827917 ) ) ;
#2087 = CARTESIAN_POINT ( 'NONE',  ( -3.164093685572913817, -79.18419798644474383, -9.628149054438361887 ) ) ;
#2088 = CARTESIAN_POINT ( 'NONE',  ( -1.070382723972096883, -126.0551519452116622, -4.385908996712817753 ) ) ;
#2089 = LINE ( 'NONE', #5313, #1990 ) ;
#2090 = AXIS2_PLACEMENT_3D ( 'NONE', #5938, #617, #13545 ) ;
#2091 = ORIENTED_EDGE ( 'NONE', *, *, #2398, .T. ) ;
#2092 = ORIENTED_EDGE ( 'NONE', *, *, #1968, .F. ) ;
#2093 = CARTESIAN_POINT ( 'NONE',  ( 53.14943414785363984, 10.84564612680554063, 2.500000000000003997 ) ) ;
#2094 = EDGE_CURVE ( 'NONE', #8094, #6099, #10548, .T. ) ;
#2095 = DIRECTION ( 'NONE',  ( -0.000000000000000000, -0.000000000000000000, -1.000000000000000000 ) ) ;
#2096 = DIRECTION ( 'NONE',  ( 0.000000000000000000, 0.000000000000000000, 1.000000000000000000 ) ) ;
#2097 = VERTEX_POINT ( 'NONE', #4224 ) ;
#2098 = CARTESIAN_POINT ( 'NONE',  ( 15.29705854078139282, 90.00000000000000000, 1.714422261702873160E-15 ) ) ;
#2099 = CIRCLE ( 'NONE', #9723, 14.99999999999998934 ) ;
#2100 = DIRECTION ( 'NONE',  ( -2.797435172181481150E-17, 1.000000000000000000, -1.765856845898762549E-18 ) ) ;
#2101 = CARTESIAN_POINT ( 'NONE',  ( 8.385254915620290461, 62.45333659073423860, 9.189312520034297072E-16 ) ) ;
#2102 = CARTESIAN_POINT ( 'NONE',  ( 39.75092559767094258, 101.0685047868945929, -2.236846530894074814 ) ) ;
#2103 = DIRECTION ( 'NONE',  ( 2.668805347656626185E-16, -1.000000000000000000, -0.000000000000000000 ) ) ;
#2104 = CARTESIAN_POINT ( 'NONE',  ( 1.032204844967210100, -126.1190415558569526, 4.386694312918715255 ) ) ;
#2105 = CARTESIAN_POINT ( 'NONE',  ( -25.00000000000000355, 120.0000000000000284, 0.5000000000000000000 ) ) ;
#2106 = ORIENTED_EDGE ( 'NONE', *, *, #13434, .F. ) ;
#2107 = ORIENTED_EDGE ( 'NONE', *, *, #792, .F. ) ;
#2108 = VERTEX_POINT ( 'NONE', #12877 ) ;
#2109 = CIRCLE ( 'NONE', #4822, 27.49999999999998579 ) ;
#2110 = CARTESIAN_POINT ( 'NONE',  ( 10.69346802281034492, 40.17406817374066463, 2.619144277183853160E-15 ) ) ;
#2111 = ORIENTED_EDGE ( 'NONE', *, *, #12193, .F. ) ;
#2112 = CARTESIAN_POINT ( 'NONE',  ( -42.16244658108818300, 105.4500712252157655, -7.500000000000000000 ) ) ;
#2113 = CARTESIAN_POINT ( 'NONE',  ( -3.926155785508803397, -105.6048756127474633, 5.752462641596377324 ) ) ;
#2114 = CARTESIAN_POINT ( 'NONE',  ( -2.889799813501109593, -137.4545454546409360, -1.105612428328569763 ) ) ;
#2115 = DIRECTION ( 'NONE',  ( 1.000000000000000000, 0.000000000000000000, 0.000000000000000000 ) ) ;
#2116 = CIRCLE ( 'NONE', #12673, 5.000000000000001776 ) ;
#2117 = CARTESIAN_POINT ( 'NONE',  ( 42.49999999999999289, 120.0000000000000142, -2.499999999999998668 ) ) ;
#2118 = CARTESIAN_POINT ( 'NONE',  ( -3.711366765501976861, -78.09090909091068511, -9.373274001092186225 ) ) ;
#2119 = EDGE_CURVE ( 'NONE', #11283, #369, #12560, .T. ) ;
#2120 = DIRECTION ( 'NONE',  ( -5.551115123125776539E-17, 1.000000000000000000, 3.944304526105059027E-31 ) ) ;
#2121 = AXIS2_PLACEMENT_3D ( 'NONE', #3251, #7526, #3314 ) ;
#2122 = FACE_OUTER_BOUND ( 'NONE', #10513, .T. ) ;
#2123 = DIRECTION ( 'NONE',  ( -6.158143864569485777E-17, -2.736152283717910599E-16, 1.000000000000000000 ) ) ;
#2124 = ORIENTED_EDGE ( 'NONE', *, *, #1564, .F. ) ;
#2125 = CARTESIAN_POINT ( 'NONE',  ( -3.915768125667399957, -76.35064935077906512, -2.796074470126640676 ) ) ;
#2126 = AXIS2_PLACEMENT_3D ( 'NONE', #12074, #3656, #1339 ) ;
#2127 = EDGE_LOOP ( 'NONE', ( #13732, #12195, #9992, #12842 ) ) ;
#2128 = DIRECTION ( 'NONE',  ( -2.797435172181481150E-17, 1.000000000000000000, -1.765856845898762549E-18 ) ) ;
#2129 = ORIENTED_EDGE ( 'NONE', *, *, #1103, .T. ) ;
#2130 = CARTESIAN_POINT ( 'NONE',  ( 25.00000000000001776, -100.0000000000000000, 7.500000000000000000 ) ) ;
#2131 = AXIS2_PLACEMENT_3D ( 'NONE', #597, #13456, #6198 ) ;
#2132 = DIRECTION ( 'NONE',  ( 0.9960067511297464593, -0.08927794634716622324, 6.802837160686558945E-17 ) ) ;
#2133 = CARTESIAN_POINT ( 'NONE',  ( 15.29705854078138927, 0.8232575913729167638, 30.59411708156278564 ) ) ;
#2134 = CARTESIAN_POINT ( 'NONE',  ( 57.42880470118691250, -62.63636363331826118, 5.311255545704360870 ) ) ;
#2135 = EDGE_CURVE ( 'NONE', #1587, #8382, #3177, .T. ) ;
#2136 = CARTESIAN_POINT ( 'NONE',  ( -26.79177319725820894, -26.24642857144861807, 4.000000000000000000 ) ) ;
#2137 = CARTESIAN_POINT ( 'NONE',  ( 15.29705854078139105, 27.21102387199583816, 1.823632900916640874E-15 ) ) ;
#2138 = DIRECTION ( 'NONE',  ( 0.000000000000000000, 1.000000000000000000, 0.000000000000000000 ) ) ;
#2139 = AXIS2_PLACEMENT_3D ( 'NONE', #4273, #7562, #7497 ) ;
#2140 = CARTESIAN_POINT ( 'NONE',  ( -35.00000000000000000, -4.286263797015736496E-15, 7.500000000000000000 ) ) ;
#2141 = DIRECTION ( 'NONE',  ( 1.000000000000000000, 0.000000000000000000, 0.000000000000000000 ) ) ;
#2142 = ADVANCED_FACE ( 'NONE', ( #5088 ), #6477, .T. ) ;
#2143 = CIRCLE ( 'NONE', #121, 5.000000000000004441 ) ;
#2144 = EDGE_CURVE ( 'NONE', #7494, #9642, #5149, .T. ) ;
#2145 = VERTEX_POINT ( 'NONE', #818 ) ;
#2146 = VECTOR ( 'NONE', #7472, 1000.000000000000000 ) ;
#2147 = CARTESIAN_POINT ( 'NONE',  ( 0.000000000000000000, 0.000000000000000000, 0.000000000000000000 ) ) ;
#2148 = ORIENTED_EDGE ( 'NONE', *, *, #5469, .F. ) ;
#2149 = CARTESIAN_POINT ( 'NONE',  ( -2.517691654963332357E-15, 90.00000000000000000, -1.589271161308885878E-16 ) ) ;
#2150 = EDGE_CURVE ( 'NONE', #7666, #1714, #11208, .T. ) ;
#2151 = CARTESIAN_POINT ( 'NONE',  ( 25.00000000000001776, -99.15310334213020838, 3.061571689641656246E-15 ) ) ;
#2152 = CARTESIAN_POINT ( 'NONE',  ( -9.723082549030324984, -72.03366437468082495, -2.708544034036612924 ) ) ;
#2153 = CARTESIAN_POINT ( 'NONE',  ( -21.99999999999999289, -97.00000000000000000, 0.000000000000000000 ) ) ;
#2154 = CIRCLE ( 'NONE', #8881, 16.99999999999998934 ) ;
#2155 = CARTESIAN_POINT ( 'NONE',  ( -35.00000000000000000, -4.286263797015736496E-15, 10.49999999999999822 ) ) ;
#2156 = ADVANCED_FACE ( 'NONE', ( #13748 ), #4093, .T. ) ;
#2157 = ORIENTED_EDGE ( 'NONE', *, *, #12861, .T. ) ;
#2158 = EDGE_CURVE ( 'NONE', #1257, #12816, #6610, .T. ) ;
#2159 = B_SPLINE_SURFACE_WITH_KNOTS ( 'NONE', 3, 3, ( 
 ( #10359, #10082, #495, #4758, #3692, #3836, #9033, #6916, #7128, #12544, #1597, #1668, #13346, #627, #6017, #7981, #563, #12259, #8121, #5953, #11403, #2646, #11203, #8186 ),
 ( #8047, #12404, #10224, #4888, #2792, #6085, #12330, #2720, #7058, #11340, #691, #4960, #12742, #3119, #3059, #8454, #8520, #7469, #5356, #11478, #6422, #53, #5162, #6158 ),
 ( #10427, #13696, #5224, #2923, #1871, #891, #9451, #9511, #4040, #9646, #6226, #3190, #12615, #13823, #11546, #2008, #962, #4170, #830, #7397, #11747, #10560, #8323, #7197 ),
 ( #8590, #5096, #9379, #11678, #7328, #10620, #2991, #1031, #4309, #7262, #2074, #6351, #6287, #1942, #13757, #10489, #11611, #4106, #5295, #12680, #9576, #13887, #2134, #4236 ) ),
 .UNSPECIFIED., .F., .F., .F.,
 ( 4, 4 ),
 ( 4, 1, 1, 1, 1, 1, 1, 1, 1, 1, 1, 1, 1, 1, 1, 1, 1, 1, 1, 1, 1, 4 ),
 ( -0.002000000000000000475, 0.02200000000000000566 ),
 ( -0.009000000000000030545, -0.004090909090909119854, -2.775557561562891043E-17, 0.0008181818181817908375, 0.005727272727272700661, 0.01250649350649347610, 0.02045454545454543360, 0.02536363636363634516, 0.03027272727272725672, 0.03518181818181816828, 0.04009090909090907984, 0.04990909090909089602, 0.05481818181818180757, 0.05972727272727271913, 0.06463636363636363069, 0.06954545454545453531, 0.07749350649350648934, 0.08427272727272726305, 0.08918181818181818155, 0.08999999999999998279, 0.09409090909090908617, 0.09900000000000000466 ),
 .UNSPECIFIED. ) ;
#2160 = VERTEX_POINT ( 'NONE', #2265 ) ;
#2161 = ORIENTED_EDGE ( 'NONE', *, *, #10712, .F. ) ;
#2162 = CARTESIAN_POINT ( 'NONE',  ( -42.16244658108818300, 105.4500712252157655, -2.499999999999999556 ) ) ;
#2163 = ORIENTED_EDGE ( 'NONE', *, *, #10211, .T. ) ;
#2164 = CARTESIAN_POINT ( 'NONE',  ( 58.17953216333035726, -10.62823074130461265, -2.500000000000000888 ) ) ;
#2165 = CARTESIAN_POINT ( 'NONE',  ( -32.50000000000000000, 110.0000000000000142, 7.500000000000000000 ) ) ;
#2166 = EDGE_CURVE ( 'NONE', #6722, #5663, #7164, .T. ) ;
#2167 = DIRECTION ( 'NONE',  ( 0.000000000000000000, 0.000000000000000000, 1.000000000000000000 ) ) ;
#2168 = DIRECTION ( 'NONE',  ( 2.797435172181479917E-17, -1.000000000000000000, 1.765856845898779112E-18 ) ) ;
#2169 = LINE ( 'NONE', #8107, #10901 ) ;
#2170 = CARTESIAN_POINT ( 'NONE',  ( -8.481997772293230042, -90.97423660740879825, 2.267516047978543448 ) ) ;
#2171 = DIRECTION ( 'NONE',  ( -1.000000000000000000, 0.000000000000000000, 0.000000000000000000 ) ) ;
#2172 = ORIENTED_EDGE ( 'NONE', *, *, #3775, .T. ) ;
#2173 = EDGE_CURVE ( 'NONE', #12949, #1257, #2227, .T. ) ;
#2174 = VERTEX_POINT ( 'NONE', #5483 ) ;
#2175 = ORIENTED_EDGE ( 'NONE', *, *, #10365, .F. ) ;
#2176 = DIRECTION ( 'NONE',  ( 1.000000000000000000, 0.000000000000000000, 0.000000000000000000 ) ) ;
#2177 = DIRECTION ( 'NONE',  ( -0.9960067511297463483, 0.08927794634716618161, -4.818676322152979407E-17 ) ) ;
#2178 = ORIENTED_EDGE ( 'NONE', *, *, #13534, .F. ) ;
#2179 = CARTESIAN_POINT ( 'NONE',  ( 10.69381717166375623, -2.714886977913000266, 2.619229793989003951E-15 ) ) ;
#2180 = CARTESIAN_POINT ( 'NONE',  ( 8.385254915620292238, 5.904668890677672088, 1.018788103988028800E-15 ) ) ;
#2181 = DIRECTION ( 'NONE',  ( 0.9960067511297463483, -0.08927794634716618161, 4.818676322152979407E-17 ) ) ;
#2182 = CARTESIAN_POINT ( 'NONE',  ( 25.00000000000001776, -100.0000000000000000, 7.500000000000000000 ) ) ;
#2183 = CARTESIAN_POINT ( 'NONE',  ( -1.652786589945713258, -148.3982683983876711, -1.815848636689608053 ) ) ;
#2184 = DIRECTION ( 'NONE',  ( 0.4545454545454531425, -0.8907235428302472391, 0.000000000000000000 ) ) ;
#2185 = DIRECTION ( 'NONE',  ( -2.797435172181481150E-17, 1.000000000000000000, -1.765856845898762549E-18 ) ) ;
#2186 = CARTESIAN_POINT ( 'NONE',  ( -9.849330193486526497, -69.00000000000014211, -1.830547125266440034 ) ) ;
#2187 = DIRECTION ( 'NONE',  ( -6.158143864569485777E-17, -2.736152283717910599E-16, 1.000000000000000000 ) ) ;
#2188 = DIRECTION ( 'NONE',  ( 1.000000000000000000, 0.000000000000000000, 0.000000000000000000 ) ) ;
#2189 = AXIS2_PLACEMENT_3D ( 'NONE', #12295, #455, #9208 ) ;
#2190 = AXIS2_PLACEMENT_3D ( 'NONE', #2235, #2298, #1259 ) ;
#2191 = DIRECTION ( 'NONE',  ( 1.000000000000000000, 0.000000000000000000, 0.000000000000000000 ) ) ;
#2192 = EDGE_LOOP ( 'NONE', ( #13564, #3313, #4409, #922 ) ) ;
#2193 = LINE ( 'NONE', #8709, #8532 ) ;
#2194 = VERTEX_POINT ( 'NONE', #108 ) ;
#2195 = CARTESIAN_POINT ( 'NONE',  ( 10.00000000000000711, 139.9999999999999716, -2.500000000000000000 ) ) ;
#2196 = EDGE_LOOP ( 'NONE', ( #5799, #7876, #226, #10586 ) ) ;
#2197 = LINE ( 'NONE', #5423, #2572 ) ;
#2198 = DIRECTION ( 'NONE',  ( -1.000000000000000000, 0.000000000000000000, 0.000000000000000000 ) ) ;
#2199 = CIRCLE ( 'NONE', #11610, 16.99999999999998934 ) ;
#2200 = CARTESIAN_POINT ( 'NONE',  ( 10.69346802281034847, 2.474956373702985601, 2.619144277183853949E-15 ) ) ;
#2201 = DIRECTION ( 'NONE',  ( -2.797435172181481150E-17, 1.000000000000000000, -1.765856845898762549E-18 ) ) ;
#2202 = CIRCLE ( 'NONE', #2886, 15.29705854078139460 ) ;
#2203 = CARTESIAN_POINT ( 'NONE',  ( -32.95454545454546746, 135.5876619995293311, 2.499999999999999556 ) ) ;
#2204 = CARTESIAN_POINT ( 'NONE',  ( 8.385254915620294014, 12.70483462268159869, 1.017890798515799537E-15 ) ) ;
#2205 = CARTESIAN_POINT ( 'NONE',  ( 39.95570474821488460, 100.9618745346225523, 2.097587229781389340 ) ) ;
#2206 = DIRECTION ( 'NONE',  ( 1.000000000000000000, 0.000000000000000000, 0.000000000000000000 ) ) ;
#2207 = LINE ( 'NONE', #2282, #8267 ) ;
#2208 = TOROIDAL_SURFACE ( 'NONE', #10924, 22.99999999999999289, 2.000000000000000000 ) ;
#2209 = EDGE_CURVE ( 'NONE', #12961, #5520, #5627, .T. ) ;
#2210 = CLOSED_SHELL ( 'NONE', ( #1193, #13062, #3042, #5170, #9600, #904, #13357, #10841, #5079, #1287, #8147, #1754, #13816, #12553, #3074, #3880, #4363, #6608, #5498, #12189, #6358, #13551, #1405, #5948, #7195, #10378, #4308, #11825, #7549, #872, #4835, #2576, #4664, #9877, #13684, #8115, #9780, #1050, #6606, #12109, #10292, #11732, #4206, #5152, #8485, #9353, #8225, #4452, #5003, #13186, #6597, #3776, #1238, #2494, #6120, #8591, #9805, #13267, #10474, #12422, #5660, #537, #12969, #8967, #8421, #11407, #7917, #71, #6262, #3412, #13662, #4752, #9281 ) ) ;
#2211 = EDGE_CURVE ( 'NONE', #5518, #3968, #1124, .T. ) ;
#2212 = SHAPE_REPRESENTATION_RELATIONSHIP ( 'NONE' , 'NONE' ,  #5134, #5722 ) ;
#2213 = ORIENTED_EDGE ( 'NONE', *, *, #12483, .T. ) ;
#2214 = PRODUCT_DEFINITION ( 'UNKNOWN', '', #1249, #3623 ) ;
#2215 = CARTESIAN_POINT ( 'NONE',  ( 38.89115197531749857, 101.6687180808697377, -2.500000000000000000 ) ) ;
#2216 = AXIS2_PLACEMENT_3D ( 'NONE', #5831, #8078, #13521 ) ;
#2217 = CARTESIAN_POINT ( 'NONE',  ( 8.385254915620285132, 53.02855864072483882, 16.77050983124058092 ) ) ;
#2218 = CARTESIAN_POINT ( 'NONE',  ( -10.00000000000000533, 92.00000000000000000, 4.500000000000000888 ) ) ;
#2219 = CARTESIAN_POINT ( 'NONE',  ( -35.00000000000000000, -4.286263797015736496E-15, -4.000000000000000000 ) ) ;
#2220 = CIRCLE ( 'NONE', #11852, 24.99999999999998934 ) ;
#2221 = CARTESIAN_POINT ( 'NONE',  ( -12.99553232110413958, 11.07475474455194053, -1.630606568990249473E-15 ) ) ;
#2222 = VERTEX_POINT ( 'NONE', #10806 ) ;
#2223 = EDGE_CURVE ( 'NONE', #10278, #7425, #10526, .T. ) ;
#2224 = AXIS2_PLACEMENT_3D ( 'NONE', #4585, #12096, #7737 ) ;
#2225 = AXIS2_PLACEMENT_3D ( 'NONE', #9848, #257, #4510 ) ;
#2226 = EDGE_CURVE ( 'NONE', #297, #5518, #12965, .T. ) ;
#2227 = CIRCLE ( 'NONE', #11455, 9.000000000008999024 ) ;
#2228 = AXIS2_PLACEMENT_3D ( 'NONE', #3934, #11506, #12497 ) ;
#2229 = VERTEX_POINT ( 'NONE', #1424 ) ;
#2230 = CARTESIAN_POINT ( 'NONE',  ( 10.11726280447958182, 5.576682675210010487, 4.336808689942017736E-16 ) ) ;
#2231 = ORIENTED_EDGE ( 'NONE', *, *, #13332, .T. ) ;
#2232 = ADVANCED_FACE ( 'NONE', ( #8780 ), #11937, .F. ) ;
#2233 = CARTESIAN_POINT ( 'NONE',  ( -25.00000000000000355, 120.0000000000000142, 2.499999999999999556 ) ) ;
#2234 = EDGE_CURVE ( 'NONE', #12385, #752, #7864, .T. ) ;
#2235 = CARTESIAN_POINT ( 'NONE',  ( 1.187907395172932673E-14, -97.00000000000000000, 0.000000000000000000 ) ) ;
#2236 = DIRECTION ( 'NONE',  ( -2.797435172181481150E-17, 1.000000000000000000, -1.765856845898762549E-18 ) ) ;
#2237 = CARTESIAN_POINT ( 'NONE',  ( 40.74280923682186284, 100.6542365527006098, -1.046903941091064327 ) ) ;
#2238 = DIRECTION ( 'NONE',  ( -1.000000000000000000, -0.000000000000000000, 0.000000000000000000 ) ) ;
#2239 = AXIS2_PLACEMENT_3D ( 'NONE', #8754, #7697, #11909 ) ;
#2240 = CARTESIAN_POINT ( 'NONE',  ( -3.789659181785903552, -84.41043748841794070, 8.773495529534001136 ) ) ;
#2241 = FACE_OUTER_BOUND ( 'NONE', #3052, .T. ) ;
#2242 = ORIENTED_EDGE ( 'NONE', *, *, #4739, .F. ) ;
#2243 = VECTOR ( 'NONE', #6352, 1000.000000000000000 ) ;
#2244 = CIRCLE ( 'NONE', #5606, 17.49999999999999289 ) ;
#2245 = ORIENTED_EDGE ( 'NONE', *, *, #12955, .F. ) ;
#2246 = VERTEX_POINT ( 'NONE', #7586 ) ;
#2247 = EDGE_CURVE ( 'NONE', #4900, #4459, #5, .T. ) ;
#2248 = DIRECTION ( 'NONE',  ( -0.000000000000000000, -0.000000000000000000, 1.000000000000000000 ) ) ;
#2249 = AXIS2_PLACEMENT_3D ( 'NONE', #4293, #6143, #1084 ) ;
#2250 = ORIENTED_EDGE ( 'NONE', *, *, #801, .F. ) ;
#2251 = DIRECTION ( 'NONE',  ( -2.797435172181481150E-17, 1.000000000000000000, -1.765856845898762549E-18 ) ) ;
#2252 = CARTESIAN_POINT ( 'NONE',  ( 12.99553232110413958, 58.19864449459908684, -25.99106464220826851 ) ) ;
#2253 = EDGE_CURVE ( 'NONE', #12007, #13310, #11863, .T. ) ;
#2254 = CIRCLE ( 'NONE', #8525, 8.385254915620294014 ) ;
#2255 = CARTESIAN_POINT ( 'NONE',  ( -10.69346802281034847, 2.474956373702985157, -1.318312975903535027E-15 ) ) ;
#2256 = VECTOR ( 'NONE', #396, 1000.000000000000000 ) ;
#2257 = DIRECTION ( 'NONE',  ( 0.000000000000000000, 1.000000000000000000, -0.000000000000000000 ) ) ;
#2258 = CARTESIAN_POINT ( 'NONE',  ( -9.736331930512843513, -69.99978782402621391, -2.722951059031194276 ) ) ;
#2259 = CARTESIAN_POINT ( 'NONE',  ( -8.152362820468885829, -73.18181818181821541, -5.943141306424241321 ) ) ;
#2260 = B_SPLINE_CURVE_WITH_KNOTS ( 'NONE', 3,
 ( #2790, #7194, #4885, #10424, #9164, #13489, #9240, #12402, #11475, #1868, #10286, #5025 ),
 .UNSPECIFIED., .F., .F.,
 ( 4, 2, 2, 2, 2, 4 ),
 ( 0.000000000000000000, 0.002041637357698527708, 0.003062456036547791995, 0.004083274715397057150, 0.006124912073095585725, 0.008166549430794116035 ),
 .UNSPECIFIED. ) ;
#2261 = DIRECTION ( 'NONE',  ( -1.000000000000000000, 0.000000000000000000, 0.000000000000000000 ) ) ;
#2262 = PLANE ( 'NONE',  #11284 ) ;
#2263 =( BOUNDED_SURFACE ( )  B_SPLINE_SURFACE ( 3, 3, ( 
 ( #11952, #58, #1438, #2343 ),
 ( #6626, #12099, #10890, #1297 ),
 ( #5563, #9853, #4513, #2413 ),
 ( #5643, #13183, #9925, #3528 ) ),
 .UNSPECIFIED., .F., .F., .F. ) 
 B_SPLINE_SURFACE_WITH_KNOTS ( ( 4, 4 ),
 ( 4, 4 ),
 ( 0.000000000000000000, 1.000000000000000000 ),
 ( 0.000000000000000000, 1.000000000000000000 ),
 .UNSPECIFIED. ) 
 GEOMETRIC_REPRESENTATION_ITEM ( )  RATIONAL_B_SPLINE_SURFACE ( (
 ( 1.000000000000000000, 0.3333333333333334259, 0.3333333333333334259, 1.000000000000000000),
 ( 1.000000000000000000, 0.3333333333333334259, 0.3333333333333334259, 1.000000000000000000),
 ( 1.000000000000000000, 0.3333333333333334259, 0.3333333333333334259, 1.000000000000000000),
 ( 1.000000000000000000, 0.3333333333333334259, 0.3333333333333334259, 1.000000000000000000) ) ) 
 REPRESENTATION_ITEM ( '' )  SURFACE ( )  );
#2264 = ORIENTED_EDGE ( 'NONE', *, *, #5545, .F. ) ;
#2265 = CARTESIAN_POINT ( 'NONE',  ( -39.99999999999999289, 120.0000000000000284, -0.5000000000000000000 ) ) ;
#2266 = PLANE ( 'NONE',  #6271 ) ;
#2267 = ORIENTED_EDGE ( 'NONE', *, *, #2144, .T. ) ;
#2268 = CARTESIAN_POINT ( 'NONE',  ( -24.99999999999998579, -99.17107372196666404, -0.8524342262974159423 ) ) ;
#2269 = DIRECTION ( 'NONE',  ( -0.000000000000000000, -0.000000000000000000, -1.000000000000000000 ) ) ;
#2270 = ORIENTED_EDGE ( 'NONE', *, *, #3722, .F. ) ;
#2271 = DIRECTION ( 'NONE',  ( 0.8907235428302473501, -0.4545454545454531425, 0.000000000000000000 ) ) ;
#2272 = EDGE_LOOP ( 'NONE', ( #10595, #6257, #8125, #2688 ) ) ;
#2273 = DIRECTION ( 'NONE',  ( 6.158143864569485777E-17, 2.736152283717910599E-16, -1.000000000000000000 ) ) ;
#2274 = CARTESIAN_POINT ( 'NONE',  ( 15.29705854078139105, 55.48535772202409078, 1.773704474924341131E-15 ) ) ;
#2275 = CARTESIAN_POINT ( 'NONE',  ( 2.449293598294706513E-15, -20.00000000000000000, -20.00000000000000000 ) ) ;
#2276 = PRODUCT_DEFINITION_SHAPE ( 'NONE', 'NONE',  #13903 ) ;
#2277 = COLOUR_RGB ( '', 0.09019608, 0.27058824, 0.51372549) ;
#2278 = CARTESIAN_POINT ( 'NONE',  ( -35.00000000000000000, -4.286263797015736496E-15, -8.499999999999998224 ) ) ;
#2279 = FACE_OUTER_BOUND ( 'NONE', #12166, .T. ) ;
#2280 = CARTESIAN_POINT ( 'NONE',  ( 39.74871155318042781, 101.0697170996391492, 2.238193420436154657 ) ) ;
#2281 = LINE ( 'NONE', #4240, #2080 ) ;
#2282 = CARTESIAN_POINT ( 'NONE',  ( 34.00000000000001421, 108.0000000000000142, 2.500000000000000000 ) ) ;
#2283 = DIRECTION ( 'NONE',  ( -1.000000000000000000, 0.000000000000000000, 0.000000000000000000 ) ) ;
#2284 = VERTEX_POINT ( 'NONE', #9836 ) ;
#2285 = ORIENTED_EDGE ( 'NONE', *, *, #5322, .T. ) ;
#2286 = ORIENTED_EDGE ( 'NONE', *, *, #5233, .F. ) ;
#2287 = CARTESIAN_POINT ( 'NONE',  ( -8.385254915620292238, 62.45333659073423860, -1.102836519679677113E-16 ) ) ;
#2288 = CARTESIAN_POINT ( 'NONE',  ( -15.29705854078138749, 17.78624592198638155, -3.140796412417860432E-17 ) ) ;
#2289 = AXIS2_PLACEMENT_3D ( 'NONE', #8458, #2078, #12747 ) ;
#2290 = LINE ( 'NONE', #67, #9034 ) ;
#2291 = DIRECTION ( 'NONE',  ( 0.9960067511297464593, -0.08927794634716622324, 3.401418580343279473E-17 ) ) ;
#2292 = ORIENTED_EDGE ( 'NONE', *, *, #5390, .T. ) ;
#2293 = ORIENTED_EDGE ( 'NONE', *, *, #368, .F. ) ;
#2294 = ORIENTED_EDGE ( 'NONE', *, *, #1730, .F. ) ;
#2295 = DIRECTION ( 'NONE',  ( -6.158143864569485777E-17, -2.736152283717910599E-16, 1.000000000000000000 ) ) ;
#2296 = ORIENTED_EDGE ( 'NONE', *, *, #7999, .T. ) ;
#2297 = CARTESIAN_POINT ( 'NONE',  ( 15.29705854078138572, 66.79670324143890525, 1.757061666260240493E-15 ) ) ;
#2298 = DIRECTION ( 'NONE',  ( -1.224646799147353207E-16, 1.000000000000000000, -0.000000000000000000 ) ) ;
#2299 = CARTESIAN_POINT ( 'NONE',  ( -34.99999999999999289, -135.0000000000000000, 0.000000000000000000 ) ) ;
#2300 = CARTESIAN_POINT ( 'NONE',  ( -34.31344059123750156, 108.0182175921208909, -1.328634118392872043 ) ) ;
#2301 = CARTESIAN_POINT ( 'NONE',  ( -15.29705854078138927, 66.79670324143890525, -3.866317875498727004E-15 ) ) ;
#2302 = ADVANCED_FACE ( 'NONE', ( #4424 ), #243, .T. ) ;
#2303 = CARTESIAN_POINT ( 'NONE',  ( 0.2804847452500967009, -81.23845599192084421, 9.920157271374822727 ) ) ;
#2304 = EDGE_CURVE ( 'NONE', #11721, #8349, #2917, .T. ) ;
#2305 = FACE_BOUND ( 'NONE', #914, .T. ) ;
#2306 = ORIENTED_EDGE ( 'NONE', *, *, #10963, .F. ) ;
#2307 = ORIENTED_EDGE ( 'NONE', *, *, #1291, .T. ) ;
#2308 = ORIENTED_EDGE ( 'NONE', *, *, #5750, .T. ) ;
#2309 = EDGE_CURVE ( 'NONE', #7723, #12373, #2452, .T. ) ;
#2310 = EDGE_CURVE ( 'NONE', #863, #11542, #10737, .T. ) ;
#2311 = AXIS2_PLACEMENT_3D ( 'NONE', #7450, #13745, #13810 ) ;
#2312 = CARTESIAN_POINT ( 'NONE',  ( 34.06230589874905235, 109.5835921350012683, -2.499999999999999112 ) ) ;
#2313 = DIRECTION ( 'NONE',  ( -0.000000000000000000, -0.000000000000000000, -1.000000000000000000 ) ) ;
#2314 = EDGE_LOOP ( 'NONE', ( #9341, #1857, #7273, #600, #10836, #5625, #2107, #3019, #266, #847 ) ) ;
#2315 = DIRECTION ( 'NONE',  ( -1.000000000000000000, -0.000000000000000000, -0.000000000000000000 ) ) ;
#2316 = SURFACE_STYLE_USAGE ( .BOTH. , #9902 ) ;
#2317 = VECTOR ( 'NONE', #10685, 1000.000000000000000 ) ;
#2318 = LINE ( 'NONE', #9686, #1241 ) ;
#2319 = DIRECTION ( 'NONE',  ( 0.000000000000000000, 0.000000000000000000, 1.000000000000000000 ) ) ;
#2320 = CARTESIAN_POINT ( 'NONE',  ( 25.00000000000001776, -100.0000000000000000, 7.500000000000000000 ) ) ;
#2321 = DIRECTION ( 'NONE',  ( -1.000000000000000000, 0.000000000000000000, 0.000000000000000000 ) ) ;
#2322 = CARTESIAN_POINT ( 'NONE',  ( -24.99999999999998934, -100.0000000000000000, 5.046127144241784990 ) ) ;
#2323 = CARTESIAN_POINT ( 'NONE',  ( 10.69346802281034847, -16.37459952631584059, 2.619144277183853555E-15 ) ) ;
#2324 = CARTESIAN_POINT ( 'NONE',  ( -35.00000000000000000, -35.00000000000000000, 7.500000000000000000 ) ) ;
#2325 = CIRCLE ( 'NONE', #3903, 25.50000000002549783 ) ;
#2326 = ORIENTED_EDGE ( 'NONE', *, *, #99, .T. ) ;
#2327 = EDGE_CURVE ( 'NONE', #10377, #430, #12102, .T. ) ;
#2328 = CARTESIAN_POINT ( 'NONE',  ( 15.29705854078139282, 74.33491362204294717, 1.740418857596141631E-15 ) ) ;
#2329 = ORIENTED_EDGE ( 'NONE', *, *, #10705, .T. ) ;
#2330 = TOROIDAL_SURFACE ( 'NONE', #3683, 48.00000000000001421, 2.000000000000000000 ) ;
#2331 = DIRECTION ( 'NONE',  ( -1.224646799147353207E-16, 1.000000000000000000, -0.000000000000000000 ) ) ;
#2332 = CARTESIAN_POINT ( 'NONE',  ( -3.554095123023855901E-16, 12.70483462268159869, -2.243491919447391838E-17 ) ) ;
#2333 = ORIENTED_EDGE ( 'NONE', *, *, #8076, .F. ) ;
#2334 = AXIS2_PLACEMENT_3D ( 'NONE', #3455, #2405, #1432 ) ;
#2335 = CARTESIAN_POINT ( 'NONE',  ( 25.00000000000000355, 120.0000000000000142, 7.500000000000000000 ) ) ;
#2336 = ORIENTED_EDGE ( 'NONE', *, *, #7773, .F. ) ;
#2337 = DIRECTION ( 'NONE',  ( -1.000000000000000000, 0.000000000000000000, 0.000000000000000000 ) ) ;
#2338 = AXIS2_PLACEMENT_3D ( 'NONE', #13400, #8030, #12309 ) ;
#2339 = DIRECTION ( 'NONE',  ( 0.9960067511297464593, -0.08927794634716622324, 3.401418580343279473E-17 ) ) ;
#2340 = CARTESIAN_POINT ( 'NONE',  ( 10.69381717166375445, 34.98422482212468054, 0.000000000000000000 ) ) ;
#2341 = CARTESIAN_POINT ( 'NONE',  ( 12.99579180576516890, 26.38439787695498495, 1.549288279656779528E-15 ) ) ;
#2342 = SHAPE_REPRESENTATION ( 'Central Body Frame & Collar', ( #8193 ), #12229 ) ;
#2343 = CARTESIAN_POINT ( 'NONE',  ( 15.29705854078140348, -29.33764382806072746, 3.746698755667525567E-15 ) ) ;
#2344 = DIRECTION ( 'NONE',  ( -2.797435172181481150E-17, 1.000000000000000000, -1.765856845898762549E-18 ) ) ;
#2345 = LINE ( 'NONE', #6357, #5557 ) ;
#2346 = VECTOR ( 'NONE', #9571, 1000.000000000000000 ) ;
#2347 = EDGE_CURVE ( 'NONE', #7744, #11376, #10158, .T. ) ;
#2348 = VERTEX_POINT ( 'NONE', #6917 ) ;
#2349 = ORIENTED_EDGE ( 'NONE', *, *, #5228, .T. ) ;
#2350 = DIRECTION ( 'NONE',  ( -0.000000000000000000, -0.000000000000000000, -1.000000000000000000 ) ) ;
#2351 = PRODUCT_CONTEXT ( 'NONE', #6296, 'mechanical' ) ;
#2352 = ORIENTED_EDGE ( 'NONE', *, *, #7375, .F. ) ;
#2353 = AXIS2_PLACEMENT_3D ( 'NONE', #10131, #5844, #11094 ) ;
#2354 = CARTESIAN_POINT ( 'NONE',  ( -8.385254915620294014, 24.75422479069652582, -4.371241731156832241E-17 ) ) ;
#2355 = CARTESIAN_POINT ( 'NONE',  ( -10.69346802281034670, 40.17406817374066463, -1.451455445216333422E-15 ) ) ;
#2356 = COLOUR_RGB ( '', 0.66274510, 0.83137255, 0.94901961) ;
#2357 = AXIS2_PLACEMENT_3D ( 'NONE', #5848, #5697, #8020 ) ;
#2358 = CARTESIAN_POINT ( 'NONE',  ( 34.99999999999958789, 1.104930248025249758E-13, -2.499999999999999112 ) ) ;
#2359 = CARTESIAN_POINT ( 'NONE',  ( -8.385254915620294014, 12.70483462268159869, -1.071767397633848135E-15 ) ) ;
#2360 = ORIENTED_EDGE ( 'NONE', *, *, #2888, .F. ) ;
#2361 = ORIENTED_EDGE ( 'NONE', *, *, #13309, .F. ) ;
#2362 = AXIS2_PLACEMENT_3D ( 'NONE', #1763, #12652, #4139 ) ;
#2363 = EDGE_CURVE ( 'NONE', #10350, #13844, #8301, .T. ) ;
#2364 = DIRECTION ( 'NONE',  ( 1.000000000000000000, -0.000000000000000000, 0.000000000000000000 ) ) ;
#2365 = ORIENTED_EDGE ( 'NONE', *, *, #5398, .T. ) ;
#2366 = CARTESIAN_POINT ( 'NONE',  ( -15.29705854078139815, 74.33491362204296138, 30.59411708156277854 ) ) ;
#2367 = DIRECTION ( 'NONE',  ( 1.000000000000000000, 0.000000000000000000, 0.000000000000000000 ) ) ;
#2368 = DIRECTION ( 'NONE',  ( -0.000000000000000000, -0.000000000000000000, -1.000000000000000000 ) ) ;
#2369 = CARTESIAN_POINT ( 'NONE',  ( -15.29705854078139282, -8.601520358636511432, 1.518905361043589440E-17 ) ) ;
#2370 = CARTESIAN_POINT ( 'NONE',  ( -0.1460947463170765848, -81.55043853261756226, 9.868234360004247918 ) ) ;
#2371 = LINE ( 'NONE', #4336, #12454 ) ;
#2372 = ORIENTED_EDGE ( 'NONE', *, *, #1041, .T. ) ;
#2373 = VERTEX_POINT ( 'NONE', #5805 ) ;
#2374 = ORIENTED_EDGE ( 'NONE', *, *, #9852, .F. ) ;
#2375 = VECTOR ( 'NONE', #4322, 1000.000000000000000 ) ;
#2376 = PRODUCT_DEFINITION_SHAPE ( 'NONE', 'NONE',  #13901 ) ;
#2377 = ADVANCED_FACE ( 'NONE', ( #9105 ), #10084, .T. ) ;
#2378 = FACE_OUTER_BOUND ( 'NONE', #12153, .T. ) ;
#2379 = EDGE_CURVE ( 'NONE', #6129, #6854, #11433, .T. ) ;
#2380 = DIRECTION ( 'NONE',  ( 6.158143864569485777E-17, 2.736152283717910599E-16, -1.000000000000000000 ) ) ;
#2381 = EDGE_LOOP ( 'NONE', ( #6923, #11451, #4968, #6883, #1090 ) ) ;
#2382 = DIRECTION ( 'NONE',  ( -6.158143864569485777E-17, -2.736152283717910599E-16, 1.000000000000000000 ) ) ;
#2383 = CARTESIAN_POINT ( 'NONE',  ( 15.29705854078138394, 36.63580182200524149, 30.59411708156277854 ) ) ;
#2384 = CARTESIAN_POINT ( 'NONE',  ( -25.00000000000000355, 120.0000000000000142, 0.5000000000000000000 ) ) ;
#2385 = CARTESIAN_POINT ( 'NONE',  ( -35.00000000000012079, 91.25000000000045475, 4.000000000000000000 ) ) ;
#2386 = DIRECTION ( 'NONE',  ( -2.797435172181481150E-17, 1.000000000000000000, -1.765856845898762549E-18 ) ) ;
#2387 = ADVANCED_FACE ( 'NONE', ( #693 ), #10580, .T. ) ;
#2388 = CARTESIAN_POINT ( 'NONE',  ( 0.5095487862222187747, -163.8787879204104456, 3.239446891907019399 ) ) ;
#2389 = CARTESIAN_POINT ( 'NONE',  ( 1.485233070515279641, -81.00000000000027001, -9.907277990170701543 ) ) ;
#2390 = DIRECTION ( 'NONE',  ( -6.158143864569485777E-17, -2.736152283717910599E-16, 1.000000000000000000 ) ) ;
#2391 = DIRECTION ( 'NONE',  ( -2.797435172181481150E-17, 1.000000000000000000, -1.765856845898762549E-18 ) ) ;
#2392 = VERTEX_POINT ( 'NONE', #3839 ) ;
#2393 = ORIENTED_EDGE ( 'NONE', *, *, #13566, .T. ) ;
#2394 = CARTESIAN_POINT ( 'NONE',  ( 34.99999999999958789, 1.091249486606660213E-13, 2.500000000000000000 ) ) ;
#2395 = DIRECTION ( 'NONE',  ( 1.000000000000000000, 0.000000000000000000, 0.000000000000000000 ) ) ;
#2396 = ORIENTED_EDGE ( 'NONE', *, *, #11180, .F. ) ;
#2397 = CARTESIAN_POINT ( 'NONE',  ( 0.000000000000000000, -100.0000000000000000, 0.000000000000000000 ) ) ;
#2398 = EDGE_CURVE ( 'NONE', #11283, #10135, #10965, .T. ) ;
#2399 = DIRECTION ( 'NONE',  ( 1.000000000000000000, 0.000000000000000000, 0.000000000000000000 ) ) ;
#2400 = FACE_OUTER_BOUND ( 'NONE', #11892, .T. ) ;
#2401 = ORIENTED_EDGE ( 'NONE', *, *, #8816, .T. ) ;
#2402 = ORIENTED_EDGE ( 'NONE', *, *, #3002, .T. ) ;
#2403 = CARTESIAN_POINT ( 'NONE',  ( -0.1852016367016632581, -70.00000000000000000, 1.488522876466137790 ) ) ;
#2404 = ORIENTED_EDGE ( 'NONE', *, *, #11143, .T. ) ;
#2405 = DIRECTION ( 'NONE',  ( -2.797435172181481150E-17, 1.000000000000000000, -1.765856845898762549E-18 ) ) ;
#2406 = CARTESIAN_POINT ( 'NONE',  ( 12.99553232110413781, 1.649976794542512337, 25.99106464220828627 ) ) ;
#2407 = CARTESIAN_POINT ( 'NONE',  ( -12.99579180576516002, 45.23395377697383424, -25.99158361153033070 ) ) ;
#2408 = EDGE_CURVE ( 'NONE', #4125, #5523, #8739, .T. ) ;
#2409 = CARTESIAN_POINT ( 'NONE',  ( 34.27497211191903403, 108.1406786207261916, -0.9834270823685519192 ) ) ;
#2410 = EDGE_CURVE ( 'NONE', #5381, #1478, #3818, .T. ) ;
#2411 = DIRECTION ( 'NONE',  ( -2.797435172181481150E-17, 1.000000000000000000, -1.765856845898762549E-18 ) ) ;
#2412 = CARTESIAN_POINT ( 'NONE',  ( -40.68412312724079527, 100.6732077982501181, -1.167148848990504639 ) ) ;
#2413 = CARTESIAN_POINT ( 'NONE',  ( 10.69381717166376333, -30.98922082794128130, 2.619229793989005134E-15 ) ) ;
#2414 = TOROIDAL_SURFACE ( 'NONE', #9155, 3.999999999999998224, 2.000000000000000000 ) ;
#2415 = DIRECTION ( 'NONE',  ( -2.797435172181481150E-17, 1.000000000000000000, -1.765856845898762549E-18 ) ) ;
#2416 = CARTESIAN_POINT ( 'NONE',  ( 10.69381717166374912, 16.13466892210585257, 21.38763434332750890 ) ) ;
#2417 = ORIENTED_EDGE ( 'NONE', *, *, #10047, .T. ) ;
#2418 = VERTEX_POINT ( 'NONE', #10360 ) ;
#2419 = VECTOR ( 'NONE', #12974, 1000.000000000000000 ) ;
#2420 = EDGE_CURVE ( 'NONE', #6795, #3901, #11215, .T. ) ;
#2421 = ORIENTED_EDGE ( 'NONE', *, *, #7901, .F. ) ;
#2422 = CARTESIAN_POINT ( 'NONE',  ( 40.00000000000000711, 100.0000000000000000, -0.5000000000000000000 ) ) ;
#2423 = VERTEX_POINT ( 'NONE', #11748 ) ;
#2424 =( BOUNDED_SURFACE ( )  B_SPLINE_SURFACE ( 3, 3, ( 
 ( #2274, #4374, #8654, #4435 ),
 ( #12953, #3320, #6557, #10815 ),
 ( #12462, #6990, #11126, #3611 ),
 ( #1512, #10279, #10215, #13481 ) ),
 .UNSPECIFIED., .F., .F., .T. ) 
 B_SPLINE_SURFACE_WITH_KNOTS ( ( 4, 4 ),
 ( 4, 4 ),
 ( 0.000000000000000000, 1.000000000000000000 ),
 ( 0.000000000000000000, 1.000000000000000000 ),
 .UNSPECIFIED. ) 
 GEOMETRIC_REPRESENTATION_ITEM ( )  RATIONAL_B_SPLINE_SURFACE ( (
 ( 1.000000000000000000, 0.3333333333333334259, 0.3333333333333334259, 1.000000000000000000),
 ( 1.000000000000000000, 0.3333333333333334259, 0.3333333333333334259, 1.000000000000000000),
 ( 1.000000000000000000, 0.3333333333333334259, 0.3333333333333334259, 1.000000000000000000),
 ( 1.000000000000000000, 0.3333333333333334259, 0.3333333333333334259, 1.000000000000000000) ) ) 
 REPRESENTATION_ITEM ( '' )  SURFACE ( )  );
#2425 = DIRECTION ( 'NONE',  ( 0.8907235428302465730, -0.4545454545454549189, 2.472254464564578633E-15 ) ) ;
#2426 = ADVANCED_FACE ( 'NONE', ( #4107 ), #2711, .T. ) ;
#2427 = FACE_OUTER_BOUND ( 'NONE', #2968, .T. ) ;
#2428 = DIRECTION ( 'NONE',  ( 1.000000000000000000, 3.558407130208836623E-15, 0.000000000000000000 ) ) ;
#2429 = VECTOR ( 'NONE', #11889, 1000.000000000000000 ) ;
#2430 = CARTESIAN_POINT ( 'NONE',  ( -14.13596196814457429, -39.17949320881311337, -1.592785305112443692E-15 ) ) ;
#2431 = VERTEX_POINT ( 'NONE', #10562 ) ;
#2432 = AXIS2_PLACEMENT_3D ( 'NONE', #13404, #2485, #12313 ) ;
#2433 = EDGE_LOOP ( 'NONE', ( #6823, #10972, #2035, #11618 ) ) ;
#2434 = CARTESIAN_POINT ( 'NONE',  ( -15.29705854078138927, 66.79670324143890525, -1.179534157023628988E-16 ) ) ;
#2435 = AXIS2_PLACEMENT_3D ( 'NONE', #6592, #4344, #5337 ) ;
#2436 = VERTEX_POINT ( 'NONE', #11479 ) ;
#2437 = ORIENTED_EDGE ( 'NONE', *, *, #2408, .F. ) ;
#2438 = DIRECTION ( 'NONE',  ( -2.797435172181481150E-17, 1.000000000000000000, -1.765856845898762549E-18 ) ) ;
#2439 = ORIENTED_EDGE ( 'NONE', *, *, #7534, .F. ) ;
#2440 = CARTESIAN_POINT ( 'NONE',  ( 0.000000000000000000, 71.01020514433645303, -0.5000000000000000000 ) ) ;
#2441 = AXIS2_PLACEMENT_3D ( 'NONE', #10480, #2981, #9370 ) ;
#2442 = DIRECTION ( 'NONE',  ( -1.000000000000000000, 0.000000000000000000, 0.000000000000000000 ) ) ;
#2443 = CARTESIAN_POINT ( 'NONE',  ( -15.29705854078139282, 36.63580182200523438, -6.469358145237827718E-17 ) ) ;
#2444 = FACE_OUTER_BOUND ( 'NONE', #1135, .T. ) ;
#2445 = DIRECTION ( 'NONE',  ( -6.158143864569485777E-17, -2.736152283717910599E-16, 1.000000000000000000 ) ) ;
#2446 = CARTESIAN_POINT ( 'NONE',  ( 12.99579180576517601, -30.16426982310158067, 1.682131806534656762E-15 ) ) ;
#2447 = FACE_OUTER_BOUND ( 'NONE', #852, .T. ) ;
#2448 = ORIENTED_EDGE ( 'NONE', *, *, #3610, .F. ) ;
#2449 = CIRCLE ( 'NONE', #1555, 24.99999999999998934 ) ;
#2450 = ORIENTED_EDGE ( 'NONE', *, *, #10971, .F. ) ;
#2451 = ORIENTED_EDGE ( 'NONE', *, *, #3896, .T. ) ;
#2452 = CIRCLE ( 'NONE', #10086, 18.74900000001875355 ) ;
#2453 = AXIS2_PLACEMENT_3D ( 'NONE', #4488, #2313, #5470 ) ;
#2454 = VERTEX_POINT ( 'NONE', #12616 ) ;
#2455 = SPHERICAL_SURFACE ( 'NONE', #10720, 5.000000000000000000 ) ;
#2456 = LINE ( 'NONE', #7710, #13496 ) ;
#2457 = ORIENTED_EDGE ( 'NONE', *, *, #5172, .F. ) ;
#2458 = FACE_OUTER_BOUND ( 'NONE', #9704, .T. ) ;
#2459 = SURFACE_STYLE_FILL_AREA ( #1480 ) ;
#2460 = DIRECTION ( 'NONE',  ( 1.000000000000000000, 0.000000000000000000, 0.000000000000000000 ) ) ;
#2461 = CARTESIAN_POINT ( 'NONE',  ( -6.999999999999999112, -35.00000000000000000, 7.500000000000000000 ) ) ;
#2462 = AXIS2_PLACEMENT_3D ( 'NONE', #7430, #7633, #6581 ) ;
#2463 = CARTESIAN_POINT ( 'NONE',  ( 5.272971512688771512, -111.2727272727264136, -4.182478603667378891 ) ) ;
#2464 = CARTESIAN_POINT ( 'NONE',  ( 37.50000000000002132, 144.4948974278317735, 7.500000000000000000 ) ) ;
#2465 = CARTESIAN_POINT ( 'NONE',  ( -15.29705854078138927, -18.02629830864593785, -30.59411708156278564 ) ) ;
#2466 = DIRECTION ( 'NONE',  ( -1.000000000000000000, 0.000000000000000000, 0.000000000000000000 ) ) ;
#2467 = VECTOR ( 'NONE', #13179, 999.9999999999998863 ) ;
#2468 = CARTESIAN_POINT ( 'NONE',  ( 0.000000000000000000, 71.01020514433645303, -0.5000000000000000000 ) ) ;
#2469 = AXIS2_PLACEMENT_3D ( 'NONE', #6078, #1728, #1661 ) ;
#2470 = CARTESIAN_POINT ( 'NONE',  ( 35.00000000000000000, 4.286263797015736496E-15, 7.500000000000000000 ) ) ;
#2471 = ADVANCED_FACE ( 'NONE', ( #7470 ), #7329, .F. ) ;
#2472 = ORIENTED_EDGE ( 'NONE', *, *, #9583, .T. ) ;
#2473 = DIRECTION ( 'NONE',  ( 0.000000000000000000, 0.000000000000000000, 1.000000000000000000 ) ) ;
#2474 = CARTESIAN_POINT ( 'NONE',  ( -32.72727272727271952, 135.1423002281142089, 2.500000000000000000 ) ) ;
#2475 = CIRCLE ( 'NONE', #12342, 9.000000000009000800 ) ;
#2476 = STYLED_ITEM ( 'NONE', ( #6796 ), #3316 ) ;
#2477 = AXIS2_PLACEMENT_3D ( 'NONE', #196, #6633, #8880 ) ;
#2478 = DIRECTION ( 'NONE',  ( 1.000000000000000000, 0.000000000000000000, 0.000000000000000000 ) ) ;
#2479 = DIRECTION ( 'NONE',  ( -2.797435172181481150E-17, 1.000000000000000000, -1.765856845898762549E-18 ) ) ;
#2480 = VERTEX_POINT ( 'NONE', #7264 ) ;
#2481 = VERTEX_POINT ( 'NONE', #2927 ) ;
#2482 = CARTESIAN_POINT ( 'NONE',  ( 0.000000000000000000, 20.00000000000000355, 0.000000000000000000 ) ) ;
#2483 = VERTEX_POINT ( 'NONE', #13697 ) ;
#2484 = CARTESIAN_POINT ( 'NONE',  ( 52.26118412238654543, 18.64354822589355365, -2.499999999999993339 ) ) ;
#2485 = DIRECTION ( 'NONE',  ( 0.000000000000000000, 1.000000000000000000, 0.000000000000000000 ) ) ;
#2486 = DIRECTION ( 'NONE',  ( -1.000000000000000000, 0.000000000000000000, 0.000000000000000000 ) ) ;
#2487 = CARTESIAN_POINT ( 'NONE',  ( 34.26147919318644597, 108.1862277804541606, -0.7448039452652778225 ) ) ;
#2488 = DIRECTION ( 'NONE',  ( -0.000000000000000000, -0.000000000000000000, -1.000000000000000000 ) ) ;
#2489 = FACE_OUTER_BOUND ( 'NONE', #3296, .T. ) ;
#2490 =( LENGTH_UNIT ( ) NAMED_UNIT ( * ) SI_UNIT ( .MILLI., .METRE. ) );
#2491 = CARTESIAN_POINT ( 'NONE',  ( -2.517691654963332357E-15, 90.00000000000000000, -1.589271161308885878E-16 ) ) ;
#2492 = TOROIDAL_SURFACE ( 'NONE', #4502, -34.24999999999974420, 69.24999999999975842 ) ;
#2493 = CARTESIAN_POINT ( 'NONE',  ( -28.79177319725820894, -26.24642857144861807, -4.000000000000000000 ) ) ;
#2494 = ADVANCED_FACE ( 'NONE', ( #8592 ), #11547, .F. ) ;
#2495 = CIRCLE ( 'NONE', #6514, 18.74900000001875000 ) ;
#2496 = SPHERICAL_SURFACE ( 'NONE', #6245, 5.000000000000000000 ) ;
#2497 = EDGE_CURVE ( 'NONE', #42, #4459, #963, .T. ) ;
#2498 = ORIENTED_EDGE ( 'NONE', *, *, #7796, .F. ) ;
#2499 = CARTESIAN_POINT ( 'NONE',  ( 25.00000000000000355, 120.0000000000000142, 0.5000000000000000000 ) ) ;
#2500 = ORIENTED_EDGE ( 'NONE', *, *, #9043, .F. ) ;
#2501 = CYLINDRICAL_SURFACE ( 'NONE', #2477, 82.49999999999998579 ) ;
#2502 = EDGE_CURVE ( 'NONE', #3802, #3703, #12744, .T. ) ;
#2503 = ADVANCED_FACE ( 'NONE', ( #9512 ), #4042, .T. ) ;
#2504 = VERTEX_POINT ( 'NONE', #6289 ) ;
#2505 = LINE ( 'NONE', #10009, #10826 ) ;
#2506 = ORIENTED_EDGE ( 'NONE', *, *, #614, .T. ) ;
#2507 = CARTESIAN_POINT ( 'NONE',  ( 15.29705854078138927, 55.48535772202409078, 1.773704474924340737E-15 ) ) ;
#2508 = CARTESIAN_POINT ( 'NONE',  ( -40.81228451836347659, 100.6358150620708471, 0.5000000000000000000 ) ) ;
#2509 = FACE_OUTER_BOUND ( 'NONE', #7236, .T. ) ;
#2510 = PRODUCT_DEFINITION_CONTEXT ( 'detailed design', #6476, 'design' ) ;
#2511 = CARTESIAN_POINT ( 'NONE',  ( 10.04421448860481370, -71.03329039087918773, 1.233851556784668180 ) ) ;
#2512 = EDGE_LOOP ( 'NONE', ( #7083, #10952, #13546, #7362 ) ) ;
#2513 = VECTOR ( 'NONE', #6343, 1000.000000000000000 ) ;
#2514 = SURFACE_SIDE_STYLE ('',( #2586 ) ) ;
#2515 = VERTEX_POINT ( 'NONE', #893 ) ;
#2516 = EDGE_CURVE ( 'NONE', #10661, #7842, #3578, .T. ) ;
#2517 = CARTESIAN_POINT ( 'NONE',  ( -12.99553232110414491, -26.62435705548577047, -3.153769166990986831E-15 ) ) ;
#2518 = ORIENTED_EDGE ( 'NONE', *, *, #13141, .T. ) ;
#2519 = SURFACE_STYLE_USAGE ( .BOTH. , #639 ) ;
#2520 = LINE ( 'NONE', #6797, #8685 ) ;
#2521 = CARTESIAN_POINT ( 'NONE',  ( 20.00023673640404098, 26.72039747452867431, 1.279702169315402704 ) ) ;
#2522 = FACE_OUTER_BOUND ( 'NONE', #493, .T. ) ;
#2523 = CARTESIAN_POINT ( 'NONE',  ( 34.25812584745457201, 108.1980041606221050, -0.5000000000000000000 ) ) ;
#2524 = DIRECTION ( 'NONE',  ( 0.9960067511297463483, -0.08927794634716618161, 4.818676322152979407E-17 ) ) ;
#2525 = VERTEX_POINT ( 'NONE', #3061 ) ;
#2526 = ORIENTED_EDGE ( 'NONE', *, *, #4312, .F. ) ;
#2527 = VECTOR ( 'NONE', #12897, 1000.000000000000000 ) ;
#2528 = EDGE_CURVE ( 'NONE', #10214, #5183, #8455, .T. ) ;
#2529 = VERTEX_POINT ( 'NONE', #10622 ) ;
#2530 = B_SPLINE_CURVE_WITH_KNOTS ( 'NONE', 3,
 ( #10089, #2430, #10161, #424 ),
 .UNSPECIFIED., .F., .F.,
 ( 4, 4 ),
 ( 0.000000000000000000, 1.000000000000000000 ),
 .UNSPECIFIED. ) ;
#2531 = DIRECTION ( 'NONE',  ( 1.601283208593975514E-16, -1.000000000000000000, 0.000000000000000000 ) ) ;
#2532 = CARTESIAN_POINT ( 'NONE',  ( 5.312266725920431476, -76.81818181818330515, 8.563072071057876045 ) ) ;
#2533 = ORIENTED_EDGE ( 'NONE', *, *, #9256, .F. ) ;
#2534 = CARTESIAN_POINT ( 'NONE',  ( 4.658052367537127481, 90.49197326372723182, 1.819943918220761514 ) ) ;
#2535 =( LENGTH_UNIT ( ) NAMED_UNIT ( * ) SI_UNIT ( .MILLI., .METRE. ) );
#2536 = DIRECTION ( 'NONE',  ( 0.000000000000000000, 0.000000000000000000, 1.000000000000000000 ) ) ;
#2537 = CARTESIAN_POINT ( 'NONE',  ( 15.29705854078139460, -18.02629830864596627, 1.906846944237139921E-15 ) ) ;
#2538 = CIRCLE ( 'NONE', #4317, 4.999999999999997335 ) ;
#2539 = DIRECTION ( 'NONE',  ( 0.9556796851544553384, -0.2944084567112177364, -2.313087999326726136E-17 ) ) ;
#2540 = DIRECTION ( 'NONE',  ( 1.067526471530071686E-16, 1.423368628706762330E-16, 1.000000000000000000 ) ) ;
#2541 = CARTESIAN_POINT ( 'NONE',  ( 7.616846500228380279, -85.78354978356603056, -7.024694013235112777 ) ) ;
#2542 = FACE_OUTER_BOUND ( 'NONE', #11453, .T. ) ;
#2543 = FACE_OUTER_BOUND ( 'NONE', #2433, .T. ) ;
#2544 = LINE ( 'NONE', #391, #7505 ) ;
#2545 = EDGE_LOOP ( 'NONE', ( #13617, #11607, #13883, #11218 ) ) ;
#2546 = ORIENTED_EDGE ( 'NONE', *, *, #3616, .F. ) ;
#2547 = ORIENTED_EDGE ( 'NONE', *, *, #12196, .F. ) ;
#2548 = CARTESIAN_POINT ( 'NONE',  ( -0.09498690616969264477, -159.7394095615612173, 1.519620673727829052 ) ) ;
#2549 = ORIENTED_EDGE ( 'NONE', *, *, #8750, .T. ) ;
#2550 = CIRCLE ( 'NONE', #10817, 14.99999999999999822 ) ;
#2551 = DIRECTION ( 'NONE',  ( -2.797435172181481150E-17, 1.000000000000000000, -1.765856845898762549E-18 ) ) ;
#2552 = CARTESIAN_POINT ( 'NONE',  ( 34.99999999999958789, 1.063887963769481123E-13, 12.50000000000000000 ) ) ;
#2553 = CYLINDRICAL_SURFACE ( 'NONE', #10635, 9.000000000008999024 ) ;
#2554 = B_SPLINE_CURVE_WITH_KNOTS ( 'NONE', 3,
 ( #386, #1212, #11013, #13226 ),
 .UNSPECIFIED., .F., .F.,
 ( 4, 4 ),
 ( 0.000000000000000000, 1.000000000000000000 ),
 .UNSPECIFIED. ) ;
#2555 = DIRECTION ( 'NONE',  ( 0.000000000000000000, 0.000000000000000000, 1.000000000000000000 ) ) ;
#2556 = VERTEX_POINT ( 'NONE', #5296 ) ;
#2557 = ORIENTED_EDGE ( 'NONE', *, *, #2166, .T. ) ;
#2558 = CARTESIAN_POINT ( 'NONE',  ( 155.9864723944028810, -111.6214737678657087, -2.500000000000000000 ) ) ;
#2559 = VERTEX_POINT ( 'NONE', #13889 ) ;
#2560 = CARTESIAN_POINT ( 'NONE',  ( 0.000000000000000000, 71.01020514433645303, 2.500000000000000000 ) ) ;
#2561 = EDGE_CURVE ( 'NONE', #4208, #8094, #7388, .T. ) ;
#2562 = CARTESIAN_POINT ( 'NONE',  ( 10.69381717166375445, 16.13466892210585613, 0.000000000000000000 ) ) ;
#2563 = AXIS2_PLACEMENT_3D ( 'NONE', #9602, #6777, #3400 ) ;
#2564 = DIRECTION ( 'NONE',  ( 0.000000000000000000, 0.000000000000000000, 1.000000000000000000 ) ) ;
#2565 = PLANE ( 'NONE',  #7747 ) ;
#2566 = DIRECTION ( 'NONE',  ( 0.000000000000000000, 0.000000000000000000, 1.000000000000000000 ) ) ;
#2567 = CARTESIAN_POINT ( 'NONE',  ( -5.503342039658565452E-16, 19.67281349139174296, -3.473937238186366113E-17 ) ) ;
#2568 = DIRECTION ( 'NONE',  ( -0.000000000000000000, 1.000000000000000000, 0.000000000000000000 ) ) ;
#2569 = VECTOR ( 'NONE', #975, 1000.000000000000000 ) ;
#2570 = ORIENTED_EDGE ( 'NONE', *, *, #11064, .T. ) ;
#2571 = CIRCLE ( 'NONE', #12204, 25.50000000002549783 ) ;
#2572 = VECTOR ( 'NONE', #12677, 1000.000000000000000 ) ;
#2573 = VERTEX_POINT ( 'NONE', #10686 ) ;
#2574 = CARTESIAN_POINT ( 'NONE',  ( 47.49999999999999289, 120.0000000000000142, -7.500000000000000000 ) ) ;
#2575 = EDGE_CURVE ( 'NONE', #769, #3876, #4714, .T. ) ;
#2576 = ADVANCED_FACE ( 'NONE', ( #56 ), #9850, .T. ) ;
#2577 = VERTEX_POINT ( 'NONE', #11812 ) ;
#2578 = DIRECTION ( 'NONE',  ( -1.000000000000000000, 0.000000000000000000, 0.000000000000000000 ) ) ;
#2579 = CARTESIAN_POINT ( 'NONE',  ( -15.29705854078138927, 57.37192529142945574, -1.013106070382630377E-16 ) ) ;
#2580 = CIRCLE ( 'NONE', #137, 3.999999999999996447 ) ;
#2581 = EDGE_CURVE ( 'NONE', #1833, #12810, #9999, .T. ) ;
#2582 = DIRECTION ( 'NONE',  ( 0.000000000000000000, 0.000000000000000000, -1.000000000000000000 ) ) ;
#2583 = CARTESIAN_POINT ( 'NONE',  ( -15.29705854078139105, -38.76242177807012723, -1.736451602112920500E-15 ) ) ;
#2584 = AXIS2_PLACEMENT_3D ( 'NONE', #13470, #1715, #12446 ) ;
#2585 = EDGE_LOOP ( 'NONE', ( #3562, #9665, #9197, #7304 ) ) ;
#2586 = SURFACE_STYLE_FILL_AREA ( #426 ) ;
#2587 = ORIENTED_EDGE ( 'NONE', *, *, #10621, .F. ) ;
#2588 = CARTESIAN_POINT ( 'NONE',  ( 15.29705854078139815, -27.45107625865536960, -30.59411708156277854 ) ) ;
#2589 = CIRCLE ( 'NONE', #5962, 79.99999999999997158 ) ;
#2590 = EDGE_CURVE ( 'NONE', #2515, #2097, #6291, .T. ) ;
#2591 = AXIS2_PLACEMENT_3D ( 'NONE', #12724, #1917, #9425 ) ;
#2592 = EDGE_CURVE ( 'NONE', #7525, #11283, #913, .T. ) ;
#2593 = ORIENTED_EDGE ( 'NONE', *, *, #8742, .F. ) ;
#2594 = CARTESIAN_POINT ( 'NONE',  ( 13.76342357120274862, 14.11587126553562221, -2.499999999999996447 ) ) ;
#2595 = CIRCLE ( 'NONE', #1464, 35.00000000000000000 ) ;
#2596 = CARTESIAN_POINT ( 'NONE',  ( -10.00000000000000000, 92.00000000000000000, -2.500000000000000000 ) ) ;
#2597 = EDGE_CURVE ( 'NONE', #2835, #10317, #7263, .T. ) ;
#2598 = DIRECTION ( 'NONE',  ( 0.7627754036039178231, -0.6466635011015234857, 0.000000000000000000 ) ) ;
#2599 = EDGE_CURVE ( 'NONE', #3638, #13463, #409, .T. ) ;
#2600 = CARTESIAN_POINT ( 'NONE',  ( -34.28525802518650067, 108.1064455385057670, 1.101804919165826790 ) ) ;
#2601 = CARTESIAN_POINT ( 'NONE',  ( -1.581702400640785156, -80.31021565580134336, -9.984810461684977767 ) ) ;
#2602 = CARTESIAN_POINT ( 'NONE',  ( -10.69346802281034670, 59.02362407375952102, -1.518026679872732817E-15 ) ) ;
#2603 = VECTOR ( 'NONE', #3421, 1000.000000000000000 ) ;
#2604 = ORIENTED_EDGE ( 'NONE', *, *, #7546, .F. ) ;
#2605 = ORIENTED_EDGE ( 'NONE', *, *, #4535, .F. ) ;
#2606 = CIRCLE ( 'NONE', #11072, 9.000000000009000800 ) ;
#2607 = CARTESIAN_POINT ( 'NONE',  ( 8.385254915620295790, -24.99427717735608212, 2.053795118489800793E-15 ) ) ;
#2608 = CARTESIAN_POINT ( 'NONE',  ( 9.849330193486522944, -69.00000000000002842, 1.830547125266435149 ) ) ;
#2609 = ORIENTED_EDGE ( 'NONE', *, *, #3276, .T. ) ;
#2610 = CARTESIAN_POINT ( 'NONE',  ( -0.3899449583696082411, -79.59552047185403012, 10.11716208309628762 ) ) ;
#2611 = AXIS2_PLACEMENT_3D ( 'NONE', #12958, #5503, #6770 ) ;
#2612 = CARTESIAN_POINT ( 'NONE',  ( 42.16244658108817589, 105.4500712252157655, 2.499999999999999556 ) ) ;
#2613 = CARTESIAN_POINT ( 'NONE',  ( 1.922734475756564121E-15, 40.00000000000000000, -15.70031846811053455 ) ) ;
#2614 = CARTESIAN_POINT ( 'NONE',  ( -10.69346802281034492, 11.89973432371241380, -1.351598593231734330E-15 ) ) ;
#2615 = CARTESIAN_POINT ( 'NONE',  ( 0.05222919907312795901, -79.03030303025963121, -10.66847369585458516 ) ) ;
#2616 = EDGE_CURVE ( 'NONE', #6810, #8462, #13314, .T. ) ;
#2617 = CARTESIAN_POINT ( 'NONE',  ( -10.00000000000000000, 90.00000000000000000, 2.500000000000000000 ) ) ;
#2618 = CARTESIAN_POINT ( 'NONE',  ( 35.00000000000000000, -4.286263797015736496E-15, -4.000000000000000000 ) ) ;
#2619 = DIRECTION ( 'NONE',  ( -6.158143864569485777E-17, -2.736152283717910599E-16, 1.000000000000000000 ) ) ;
#2620 = ORIENTED_EDGE ( 'NONE', *, *, #4650, .F. ) ;
#2621 = VERTEX_POINT ( 'NONE', #3257 ) ;
#2622 = VECTOR ( 'NONE', #12188, 1000.000000000000000 ) ;
#2623 = CARTESIAN_POINT ( 'NONE',  ( 35.00000000000001421, -34.99999999999999289, 7.500000000000000000 ) ) ;
#2624 = ORIENTED_EDGE ( 'NONE', *, *, #628, .F. ) ;
#2625 = CARTESIAN_POINT ( 'NONE',  ( 2.607973140908031784, -104.0364159275374760, -6.664989919102580984 ) ) ;
#2626 = CARTESIAN_POINT ( 'NONE',  ( -15.29705854078138927, 29.09759144140119957, -5.138218104596347907E-17 ) ) ;
#2627 = DIRECTION ( 'NONE',  ( -2.797435172181481150E-17, 1.000000000000000000, -1.765856845898762549E-18 ) ) ;
#2628 = ORIENTED_EDGE ( 'NONE', *, *, #124, .T. ) ;
#2629 = ORIENTED_EDGE ( 'NONE', *, *, #7360, .F. ) ;
#2630 = DIRECTION ( 'NONE',  ( -1.000000000000000000, 0.000000000000000000, 0.000000000000000000 ) ) ;
#2631 = VERTEX_POINT ( 'NONE', #186 ) ;
#2632 = CARTESIAN_POINT ( 'NONE',  ( -0.5090839304981049640, -157.9207379528257604, -1.416845878072839460 ) ) ;
#2633 = DIRECTION ( 'NONE',  ( -6.158143864569485777E-17, -2.736152283717910599E-16, 1.000000000000000000 ) ) ;
#2634 = DIRECTION ( 'NONE',  ( -6.158143864569485777E-17, -2.736152283717910599E-16, 1.000000000000000000 ) ) ;
#2635 = DIRECTION ( 'NONE',  ( 0.1928999275155751925, 0.9812184353977893014, 2.891205793291787151E-16 ) ) ;
#2636 = DIRECTION ( 'NONE',  ( -6.158143864569485777E-17, -2.736152283717910599E-16, 1.000000000000000000 ) ) ;
#2637 = CARTESIAN_POINT ( 'NONE',  ( 12.99553232110414491, -7.774801155466914970, 0.000000000000000000 ) ) ;
#2638 = ORIENTED_EDGE ( 'NONE', *, *, #6959, .T. ) ;
#2639 = DIRECTION ( 'NONE',  ( -2.797435172181481150E-17, 1.000000000000000000, -1.765856845898762549E-18 ) ) ;
#2640 = AXIS2_PLACEMENT_3D ( 'NONE', #7358, #3152, #1066 ) ;
#2641 = VERTEX_POINT ( 'NONE', #7532 ) ;
#2642 = CARTESIAN_POINT ( 'NONE',  ( 2.920448137081741891, -118.2727272727312595, 4.227847206581237138 ) ) ;
#2643 = ORIENTED_EDGE ( 'NONE', *, *, #12535, .T. ) ;
#2644 = FACE_OUTER_BOUND ( 'NONE', #1184, .T. ) ;
#2645 = SHAPE_DEFINITION_REPRESENTATION ( #5400, #12318 ) ;
#2646 = CARTESIAN_POINT ( 'NONE',  ( 5.849706340539694516, -65.63636363268138041, 2.546235460329709710 ) ) ;
#2647 = CARTESIAN_POINT ( 'NONE',  ( -10.69381717166375800, 6.709890972096425266, 21.38763434332750890 ) ) ;
#2648 = CARTESIAN_POINT ( 'NONE',  ( -15.29705854078140348, -19.91286587805129926, 30.59411708156278564 ) ) ;
#2649 = CARTESIAN_POINT ( 'NONE',  ( 10.69346802281034847, -35.22415542633469698, 2.619144277183853555E-15 ) ) ;
#2650 = CARTESIAN_POINT ( 'NONE',  ( 14.13596196814457606, -39.17949320881311337, 3.462312115431394170E-15 ) ) ;
#2651 = CARTESIAN_POINT ( 'NONE',  ( 34.99999999999958789, 1.091249486606660213E-13, 2.500000000000000000 ) ) ;
#2652 = ORIENTED_EDGE ( 'NONE', *, *, #4385, .F. ) ;
#2653 = EDGE_CURVE ( 'NONE', #863, #9139, #8087, .T. ) ;
#2654 = CIRCLE ( 'NONE', #2189, 2.000000000000003997 ) ;
#2655 = ORIENTED_EDGE ( 'NONE', *, *, #3503, .T. ) ;
#2656 = VECTOR ( 'NONE', #12777, 1000.000000000000000 ) ;
#2657 = DIRECTION ( 'NONE',  ( -0.000000000000000000, -0.000000000000000000, -1.000000000000000000 ) ) ;
#2658 = ORIENTED_EDGE ( 'NONE', *, *, #11315, .T. ) ;
#2659 = DIRECTION ( 'NONE',  ( 0.000000000000000000, 0.000000000000000000, 1.000000000000000000 ) ) ;
#2660 = AXIS2_PLACEMENT_3D ( 'NONE', #10823, #191, #1299 ) ;
#2661 = DIRECTION ( 'NONE',  ( -2.797435172181481150E-17, 1.000000000000000000, -1.765856845898762549E-18 ) ) ;
#2662 = DIRECTION ( 'NONE',  ( 0.000000000000000000, 0.000000000000000000, 1.000000000000000000 ) ) ;
#2663 = CARTESIAN_POINT ( 'NONE',  ( -34.26155123102907396, 108.1859746833188041, -0.7471162051235282764 ) ) ;
#2664 = CARTESIAN_POINT ( 'NONE',  ( 2.866591608029287919, -101.4961736542552160, 6.904028388510872638 ) ) ;
#2665 = CARTESIAN_POINT ( 'NONE',  ( -10.69381717166376156, -30.98922082794128130, -2.584341753958642254E-15 ) ) ;
#2666 = ORIENTED_EDGE ( 'NONE', *, *, #3262, .T. ) ;
#2667 = ADVANCED_FACE ( 'NONE', ( #11950 ), #5426, .T. ) ;
#2668 = ORIENTED_EDGE ( 'NONE', *, *, #9951, .F. ) ;
#2669 = EDGE_CURVE ( 'NONE', #13011, #3550, #2926, .T. ) ;
#2670 = AXIS2_PLACEMENT_3D ( 'NONE', #4014, #6327, #1073 ) ;
#2671 = CARTESIAN_POINT ( 'NONE',  ( 34.99999999999958789, 1.091249486606660213E-13, 2.500000000000000000 ) ) ;
#2672 = EDGE_CURVE ( 'NONE', #13647, #8899, #5165, .T. ) ;
#2673 = EDGE_CURVE ( 'NONE', #8113, #42, #9191, .T. ) ;
#2674 = ORIENTED_EDGE ( 'NONE', *, *, #1830, .T. ) ;
#2675 = DIRECTION ( 'NONE',  ( 0.000000000000000000, 1.000000000000000000, 0.000000000000000000 ) ) ;
#2676 = CARTESIAN_POINT ( 'NONE',  ( -23.09891356890233993, -97.97864346908494326, 7.500000000000000000 ) ) ;
#2677 = ORIENTED_EDGE ( 'NONE', *, *, #1191, .F. ) ;
#2678 = CARTESIAN_POINT ( 'NONE',  ( -15.29705854078139637, 64.91013567203349055, -1.146220074446778111E-16 ) ) ;
#2679 = FILL_AREA_STYLE ('',( #9200 ) ) ;
#2680 = CARTESIAN_POINT ( 'NONE',  ( -22.00000000000000000, -35.00000000000000000, 7.500000000000000000 ) ) ;
#2681 = CARTESIAN_POINT ( 'NONE',  ( 5.770059030975414061, -111.2727272727274510, -3.008649887262795808 ) ) ;
#2682 = CARTESIAN_POINT ( 'NONE',  ( -10.69381717166375800, 44.40900277213413716, 21.38763434332750535 ) ) ;
#2683 = CARTESIAN_POINT ( 'NONE',  ( 9.846850911383061344, -91.60173160173981444, -0.3733502116074404742 ) ) ;
#2684 = CYLINDRICAL_SURFACE ( 'NONE', #1034, 20.00000000000000000 ) ;
#2685 = AXIS2_PLACEMENT_3D ( 'NONE', #13873, #11664, #9292 ) ;
#2686 = LINE ( 'NONE', #4717, #6238 ) ;
#2687 = DIRECTION ( 'NONE',  ( 0.7999999999999999334, -0.6000000000000001998, 0.000000000000000000 ) ) ;
#2688 = ORIENTED_EDGE ( 'NONE', *, *, #892, .F. ) ;
#2689 = ORIENTED_EDGE ( 'NONE', *, *, #8985, .T. ) ;
#2690 = AXIS2_PLACEMENT_3D ( 'NONE', #11538, #9299, #3967 ) ;
#2691 = EDGE_CURVE ( 'NONE', #1421, #1176, #5843, .T. ) ;
#2692 = DIRECTION ( 'NONE',  ( -0.7328050451781167318, -0.6804386568688601811, -2.409338161076489703E-16 ) ) ;
#2693 = EDGE_LOOP ( 'NONE', ( #13345, #7689, #6148, #5706 ) ) ;
#2694 = CARTESIAN_POINT ( 'NONE',  ( -2.021131906156611535, -99.55200189714852854, -7.478639190186810559 ) ) ;
#2695 = DIRECTION ( 'NONE',  ( -0.000000000000000000, -0.000000000000000000, 1.000000000000000000 ) ) ;
#2696 = CARTESIAN_POINT ( 'NONE',  ( 8.385254915620294014, 12.70483462268159869, 1.002145295323929345E-15 ) ) ;
#2697 = EDGE_CURVE ( 'NONE', #2418, #3001, #247, .T. ) ;
#2699 = CIRCLE ( 'NONE', #4462, 15.29705854078138927 ) ;
#2698 = CARTESIAN_POINT ( 'NONE',  ( 39.08445607832919677, 20.74481184150345214, -2.499999999999992895 ) ) ;
#2700 = AXIS2_PLACEMENT_3D ( 'NONE', #5599, #11709, #14 ) ;
#2701 = CARTESIAN_POINT ( 'NONE',  ( 25.00000000000000355, 120.0000000000000142, 7.500000000000000000 ) ) ;
#2702 = DIRECTION ( 'NONE',  ( -6.158143864569485777E-17, -2.736152283717910599E-16, 1.000000000000000000 ) ) ;
#2703 = CARTESIAN_POINT ( 'NONE',  ( 3.598469168196945844, -133.8876842431320142, 0.1837403886752023985 ) ) ;
#2704 = AXIS2_PLACEMENT_3D ( 'NONE', #5719, #8878, #7816 ) ;
#2705 = VECTOR ( 'NONE', #7761, 1000.000000000000000 ) ;
#2706 = CARTESIAN_POINT ( 'NONE',  ( 4.895553837162434974, 90.06565955263931755, -1.025098571782897983 ) ) ;
#2707 = DIRECTION ( 'NONE',  ( -0.4545454545454548634, 0.8907235428302464619, 0.000000000000000000 ) ) ;
#2708 = DIRECTION ( 'NONE',  ( -1.000000000000000000, -5.171946152600902986E-17, 0.000000000000000000 ) ) ;
#2709 = CARTESIAN_POINT ( 'NONE',  ( -0.1852016367018560761, -70.00000000000000000, 1.488522876466114253 ) ) ;
#2710 = CARTESIAN_POINT ( 'NONE',  ( -12.99579180576517246, 64.08350967699263379, -1.817850092276246042E-15 ) ) ;
#2711 = TOROIDAL_SURFACE ( 'NONE', #695, 42.00000000000001421, 2.000000000000000000 ) ;
#2712 = ORIENTED_EDGE ( 'NONE', *, *, #7531, .T. ) ;
#2713 = CARTESIAN_POINT ( 'NONE',  ( 4.330127018922190096, 91.83037361138187293, 2.500000000000000000 ) ) ;
#2714 = ORIENTED_EDGE ( 'NONE', *, *, #9894, .F. ) ;
#2715 = CARTESIAN_POINT ( 'NONE',  ( -3.042673274263591132, -100.2727272727296537, -12.70187379131512628 ) ) ;
#2716 = VERTEX_POINT ( 'NONE', #476 ) ;
#2717 = CARTESIAN_POINT ( 'NONE',  ( 2.449293598294706513E-15, -20.00000000000000000, -20.00000000000000000 ) ) ;
#2718 = DIRECTION ( 'NONE',  ( -1.224646799147353207E-16, 1.000000000000000000, -0.000000000000000000 ) ) ;
#2719 = AXIS2_PLACEMENT_3D ( 'NONE', #11729, #2058, #12667 ) ;
#2720 = CARTESIAN_POINT ( 'NONE',  ( 3.056920711447597139, -140.5584415584316957, 3.800163123442064528 ) ) ;
#2721 = AXIS2_PLACEMENT_3D ( 'NONE', #3215, #9884, #286 ) ;
#2722 = VECTOR ( 'NONE', #12127, 999.9999999999998863 ) ;
#2723 = DIRECTION ( 'NONE',  ( -2.797435172181481150E-17, 1.000000000000000000, -1.765856845898762549E-18 ) ) ;
#2724 = CARTESIAN_POINT ( 'NONE',  ( 12.99579180576517423, -20.73949187309215247, 3.183050967463144168E-15 ) ) ;
#2725 = CARTESIAN_POINT ( 'NONE',  ( 12.99553232110413425, -36.04913500549519512, 25.99106464220827917 ) ) ;
#2726 = CARTESIAN_POINT ( 'NONE',  ( 8.235865160261019113, -74.54711633044367147, 5.866162657818820847 ) ) ;
#2727 = B_SPLINE_CURVE_WITH_KNOTS ( 'NONE', 3,
 ( #8863, #8943, #7731, #10812 ),
 .UNSPECIFIED., .F., .F.,
 ( 4, 4 ),
 ( 0.000000000000000000, 1.000000000000000000 ),
 .UNSPECIFIED. ) ;
#2728 = ORIENTED_EDGE ( 'NONE', *, *, #6920, .F. ) ;
#2729 = VERTEX_POINT ( 'NONE', #1719 ) ;
#2730 =( BOUNDED_SURFACE ( )  B_SPLINE_SURFACE ( 3, 3, ( 
 ( #7377, #11386, #11597, #13808 ),
 ( #13743, #3891, #4088, #5082 ),
 ( #1780, #4158, #1989, #9364 ),
 ( #6270, #8440, #12729, #2840 ) ),
 .UNSPECIFIED., .F., .F., .F. ) 
 B_SPLINE_SURFACE_WITH_KNOTS ( ( 4, 4 ),
 ( 4, 4 ),
 ( 0.000000000000000000, 1.000000000000000000 ),
 ( 0.000000000000000000, 1.000000000000000000 ),
 .UNSPECIFIED. ) 
 GEOMETRIC_REPRESENTATION_ITEM ( )  RATIONAL_B_SPLINE_SURFACE ( (
 ( 1.000000000000000000, 0.3333333333333334259, 0.3333333333333334259, 1.000000000000000000),
 ( 1.000000000000000000, 0.3333333333333334259, 0.3333333333333334259, 1.000000000000000000),
 ( 1.000000000000000000, 0.3333333333333334259, 0.3333333333333334259, 1.000000000000000000),
 ( 1.000000000000000000, 0.3333333333333334259, 0.3333333333333334259, 1.000000000000000000) ) ) 
 REPRESENTATION_ITEM ( '' )  SURFACE ( )  );
#2731 = AXIS2_PLACEMENT_3D ( 'NONE', #7513, #9360, #1008 ) ;
#2732 = B_SPLINE_CURVE_WITH_KNOTS ( 'NONE', 3,
 ( #7890, #6841, #1363, #13180 ),
 .UNSPECIFIED., .F., .F.,
 ( 4, 4 ),
 ( 0.000000000000000000, 1.000000000000000000 ),
 .UNSPECIFIED. ) ;
#2733 = CARTESIAN_POINT ( 'NONE',  ( 15.29705854078139637, -27.45107625865536605, 1.949638918210572832E-15 ) ) ;
#2734 = EDGE_LOOP ( 'NONE', ( #1243, #12687, #10659, #9162 ) ) ;
#2735 = ORIENTED_EDGE ( 'NONE', *, *, #2597, .F. ) ;
#2736 = CARTESIAN_POINT ( 'NONE',  ( 8.385254915620301119, -34.41905512736551032, -16.77050983124059158 ) ) ;
#2737 = EDGE_CURVE ( 'NONE', #2641, #3010, #8073, .T. ) ;
#2738 = DIRECTION ( 'NONE',  ( -1.224646799147353207E-16, 1.000000000000000000, -0.000000000000000000 ) ) ;
#2739 = DIRECTION ( 'NONE',  ( -6.158143864569485777E-17, -2.736152283717910599E-16, 1.000000000000000000 ) ) ;
#2740 = DIRECTION ( 'NONE',  ( -1.000000000000000000, 0.000000000000000000, 0.000000000000000000 ) ) ;
#2741 = CARTESIAN_POINT ( 'NONE',  ( 5.802558726164779301, -86.30923214627286200, -7.334200378339981619 ) ) ;
#2742 = CARTESIAN_POINT ( 'NONE',  ( 10.69346802281033781, 59.02362407375952102, 21.38693604562068984 ) ) ;
#2743 = VERTEX_POINT ( 'NONE', #6982 ) ;
#2744 = VERTEX_POINT ( 'NONE', #1655 ) ;
#2745 = CARTESIAN_POINT ( 'NONE',  ( -25.00000000000000355, 120.0000000000000142, 0.5000000000000000000 ) ) ;
#2746 = CARTESIAN_POINT ( 'NONE',  ( 2.197875741315407971, -79.21212121212158763, 9.798460318839140371 ) ) ;
#2747 = ORIENTED_EDGE ( 'NONE', *, *, #6781, .F. ) ;
#2748 = CARTESIAN_POINT ( 'NONE',  ( 9.243399941159408328, -71.03723844962674150, 4.118320456981444444 ) ) ;
#2749 = EDGE_CURVE ( 'NONE', #11361, #6776, #2018, .T. ) ;
#2750 = CARTESIAN_POINT ( 'NONE',  ( 2.264596963715684641, -106.9090909090917449, -6.916633125700833773 ) ) ;
#2751 = CARTESIAN_POINT ( 'NONE',  ( -10.00000000000000711, 139.9999999999999716, 0.5000000000000000000 ) ) ;
#2752 = DIRECTION ( 'NONE',  ( 0.000000000000000000, 0.000000000000000000, 1.000000000000000000 ) ) ;
#2753 = CARTESIAN_POINT ( 'NONE',  ( 1.024176664970867456, -142.5800865801970758, 2.358741788133955186 ) ) ;
#2754 = CYLINDRICAL_SURFACE ( 'NONE', #10212, 9.000000000008999024 ) ;
#2755 = B_SPLINE_CURVE_WITH_KNOTS ( 'NONE', 3,
 ( #8424, #728, #10519, #9411, #9269, #9480, #13655, #10589, #3028, #9546, #13788, #1837, #10459, #7159, #13855, #4073 ),
 .UNSPECIFIED., .F., .F.,
 ( 4, 2, 2, 2, 2, 2, 2, 4 ),
 ( 0.000000000000000000, 0.003943481679486457968, 0.005915222519229687385, 0.007886963358972917670, 0.009858704198716147088, 0.01183044503845937477, 0.01380218587820260419, 0.01577392671794583534 ),
 .UNSPECIFIED. ) ;
#2756 = VECTOR ( 'NONE', #8329, 1000.000000000000000 ) ;
#2757 = CARTESIAN_POINT ( 'NONE',  ( -15.29705854078139282, 36.63580182200523438, -6.469358145237827718E-17 ) ) ;
#2758 = ADVANCED_FACE ( 'NONE', ( #8171 ), #1924, .T. ) ;
#2759 = AXIS2_PLACEMENT_3D ( 'NONE', #2567, #8875, #6844 ) ;
#2760 =( LENGTH_UNIT ( ) NAMED_UNIT ( * ) SI_UNIT ( .MILLI., .METRE. ) );
#2761 = EDGE_CURVE ( 'NONE', #6483, #7762, #11124, .T. ) ;
#2762 = VERTEX_POINT ( 'NONE', #10735 ) ;
#2763 = EDGE_LOOP ( 'NONE', ( #2604, #4999, #10793, #5861, #7324, #5018, #13356, #5893, #11172, #9843 ) ) ;
#2764 = ORIENTED_EDGE ( 'NONE', *, *, #12628, .F. ) ;
#2765 = LINE ( 'NONE', #4864, #12584 ) ;
#2766 = EDGE_LOOP ( 'NONE', ( #12928, #8220 ) ) ;
#2767 = CARTESIAN_POINT ( 'NONE',  ( -3.600965394138023523, -133.8702908180223119, -0.1741706324120513294 ) ) ;
#2768 = PLANE ( 'NONE',  #8279 ) ;
#2769 = DIRECTION ( 'NONE',  ( -6.158143864569485777E-17, -2.736152283717910599E-16, 1.000000000000000000 ) ) ;
#2770 = CIRCLE ( 'NONE', #10797, 16.99999999999998934 ) ;
#2771 = DIRECTION ( 'NONE',  ( -6.158143864569485777E-17, -2.736152283717910599E-16, 1.000000000000000000 ) ) ;
#2772 = ORIENTED_EDGE ( 'NONE', *, *, #5963, .F. ) ;
#2773 = LINE ( 'NONE', #544, #2804 ) ;
#2774 = CARTESIAN_POINT ( 'NONE',  ( 3.636509701354637691, -131.0710334046880234, -1.453205936098713735 ) ) ;
#2775 = DIRECTION ( 'NONE',  ( 2.797435172181480534E-17, -1.000000000000000000, 1.765856845898762164E-18 ) ) ;
#2776 = CYLINDRICAL_SURFACE ( 'NONE', #10301, 15.29705854078138927 ) ;
#2777 = CARTESIAN_POINT ( 'NONE',  ( -4.974937185533102380, 90.00000000000000000, -0.5000000000000000000 ) ) ;
#2778 = AXIS2_PLACEMENT_3D ( 'NONE', #11087, #11300, #653 ) ;
#2779 = DIRECTION ( 'NONE',  ( -0.000000000000000000, -0.000000000000000000, -1.000000000000000000 ) ) ;
#2780 = AXIS2_PLACEMENT_3D ( 'NONE', #9766, #10741, #7656 ) ;
#2781 = EDGE_CURVE ( 'NONE', #3080, #3209, #11999, .T. ) ;
#2782 = ORIENTED_EDGE ( 'NONE', *, *, #1772, .F. ) ;
#2783 = CARTESIAN_POINT ( 'NONE',  ( -2.237684797877294057E-15, 79.99058638175036151, -1.412519245696701404E-16 ) ) ;
#2784 = ORIENTED_EDGE ( 'NONE', *, *, #122, .T. ) ;
#2785 = DIRECTION ( 'NONE',  ( 1.000000000000000000, 0.000000000000000000, 0.000000000000000000 ) ) ;
#2786 = ORIENTED_EDGE ( 'NONE', *, *, #7997, .F. ) ;
#2787 = ORIENTED_EDGE ( 'NONE', *, *, #13704, .T. ) ;
#2788 = AXIS2_PLACEMENT_3D ( 'NONE', #1447, #3468, #4754 ) ;
#2789 = DIRECTION ( 'NONE',  ( -1.000000000000000000, 0.000000000000000000, 0.000000000000000000 ) ) ;
#2790 = CARTESIAN_POINT ( 'NONE',  ( -15.18222645069203303, -16.04698886238941924, -4.000000000000000000 ) ) ;
#2791 = EDGE_CURVE ( 'NONE', #13463, #6241, #1801, .T. ) ;
#2792 = CARTESIAN_POINT ( 'NONE',  ( -4.208314830420946784, -157.8181818182383438, -0.6624707635850120013 ) ) ;
#2793 = DIRECTION ( 'NONE',  ( 1.000000000000000000, 3.636937494461720708E-15, 0.000000000000000000 ) ) ;
#2794 = CARTESIAN_POINT ( 'NONE',  ( -40.81228451836656745, 100.6358150620699519, 0.7758357214534903346 ) ) ;
#2795 = EDGE_CURVE ( 'NONE', #5632, #5338, #5591, .T. ) ;
#2796 = LINE ( 'NONE', #633, #4094 ) ;
#2797 = CARTESIAN_POINT ( 'NONE',  ( 32.50000000000000000, 4.286263797015736496E-15, 7.500000000000000000 ) ) ;
#2798 = VECTOR ( 'NONE', #3187, 1000.000000000000000 ) ;
#2799 = VERTEX_POINT ( 'NONE', #527 ) ;
#2800 = DIRECTION ( 'NONE',  ( 0.000000000000000000, 0.000000000000000000, 1.000000000000000000 ) ) ;
#2801 = ORIENTED_EDGE ( 'NONE', *, *, #7321, .F. ) ;
#2802 = CARTESIAN_POINT ( 'NONE',  ( -12.99579180576517246, -20.73949187309215247, -3.174617675444691075E-15 ) ) ;
#2803 = CYLINDRICAL_SURFACE ( 'NONE', #866, 31.93204061526060045 ) ;
#2804 = VECTOR ( 'NONE', #1848, 1000.000000000000227 ) ;
#2805 = CARTESIAN_POINT ( 'NONE',  ( 12.99579180576516713, -1.889935973073297859, 1.604750804297411238E-15 ) ) ;
#2806 = DIRECTION ( 'NONE',  ( -1.000000000000000000, 0.000000000000000000, 0.000000000000000000 ) ) ;
#2807 = CARTESIAN_POINT ( 'NONE',  ( -5.569711040290264314, -116.8635738538862654, -0.6440865148614328684 ) ) ;
#2808 = CARTESIAN_POINT ( 'NONE',  ( 12.99553232110412893, 58.19864449459908684, 25.99106464220827561 ) ) ;
#2809 =( BOUNDED_SURFACE ( )  B_SPLINE_SURFACE ( 3, 3, ( 
 ( #11225, #1615, #5900, #10173 ),
 ( #584, #4847, #13438, #5972 ),
 ( #1956, #10444, #8341, #11426 ),
 ( #980, #12635, #4060, #3075 ) ),
 .UNSPECIFIED., .F., .F., .T. ) 
 B_SPLINE_SURFACE_WITH_KNOTS ( ( 4, 4 ),
 ( 4, 4 ),
 ( 0.000000000000000000, 1.000000000000000000 ),
 ( 0.000000000000000000, 1.000000000000000000 ),
 .UNSPECIFIED. ) 
 GEOMETRIC_REPRESENTATION_ITEM ( )  RATIONAL_B_SPLINE_SURFACE ( (
 ( 1.000000000000000000, 0.3333333333333334259, 0.3333333333333334259, 1.000000000000000000),
 ( 1.000000000000000000, 0.3333333333333334259, 0.3333333333333334259, 1.000000000000000000),
 ( 1.000000000000000000, 0.3333333333333334259, 0.3333333333333334259, 1.000000000000000000),
 ( 1.000000000000000000, 0.3333333333333334259, 0.3333333333333334259, 1.000000000000000000) ) ) 
 REPRESENTATION_ITEM ( '' )  SURFACE ( )  );
#2810 = ORIENTED_EDGE ( 'NONE', *, *, #3408, .F. ) ;
#2811 = CIRCLE ( 'NONE', #585, 14.99999999999999112 ) ;
#2812 = DIRECTION ( 'NONE',  ( 0.8000000000000012657, -0.5999999999999982014, 0.000000000000000000 ) ) ;
#2813 = CIRCLE ( 'NONE', #10639, 1.999999999999998890 ) ;
#2814 = CARTESIAN_POINT ( 'NONE',  ( -12.99553232110414491, -26.62435705548577047, -1.497464099677451275E-15 ) ) ;
#2815 = CARTESIAN_POINT ( 'NONE',  ( 3.711366765502052356, -78.09090909090807031, 9.373274001092589458 ) ) ;
#2816 = EDGE_LOOP ( 'NONE', ( #2293, #4955, #8610, #1789 ) ) ;
#2817 = CARTESIAN_POINT ( 'NONE',  ( 3.108119077941494446, -77.10324909055569265, 9.630131019297053285 ) ) ;
#2818 = DIRECTION ( 'NONE',  ( 0.000000000000000000, 0.000000000000000000, 1.000000000000000000 ) ) ;
#2819 = AXIS2_PLACEMENT_3D ( 'NONE', #4004, #11369, #5988 ) ;
#2820 = CARTESIAN_POINT ( 'NONE',  ( -5.272971512688663154, -111.2727272727274368, 4.182478603667165729 ) ) ;
#2821 = CYLINDRICAL_SURFACE ( 'NONE', #4150, 8.385254915620292238 ) ;
#2822 = CARTESIAN_POINT ( 'NONE',  ( -12.99553232110414314, 20.49953269456136695, -1.663892186318449368E-15 ) ) ;
#2823 = CARTESIAN_POINT ( 'NONE',  ( 0.1852016367012860043, -160.0000000000003126, -1.488522876466233713 ) ) ;
#2824 = CIRCLE ( 'NONE', #1934, 15.29705854078139105 ) ;
#2825 = VERTEX_POINT ( 'NONE', #9976 ) ;
#2826 = ADVANCED_FACE ( 'NONE', ( #1485 ), #9577, .T. ) ;
#2827 = VERTEX_POINT ( 'NONE', #10183 ) ;
#2828 = CARTESIAN_POINT ( 'NONE',  ( 1.787228567177412186, -149.6910924273273906, -0.8766906025594750629 ) ) ;
#2829 = VERTEX_POINT ( 'NONE', #12225 ) ;
#2830 = EDGE_CURVE ( 'NONE', #4611, #5338, #7408, .T. ) ;
#2831 = CARTESIAN_POINT ( 'NONE',  ( -3.430185293861314655, -134.8221474816296563, -0.6797513324038796378 ) ) ;
#2832 = EDGE_CURVE ( 'NONE', #8984, #13646, #5895, .T. ) ;
#2833 = CARTESIAN_POINT ( 'NONE',  ( 27.45605056404223987, 17.16431845161426040, -2.499999999999994671 ) ) ;
#2834 = DIRECTION ( 'NONE',  ( -2.797435172181481150E-17, 1.000000000000000000, -1.765856845898762549E-18 ) ) ;
#2835 = VERTEX_POINT ( 'NONE', #6952 ) ;
#2836 = FACE_OUTER_BOUND ( 'NONE', #4704, .T. ) ;
#2837 = CARTESIAN_POINT ( 'NONE',  ( -13.79311422413708499, -21.62638421600851046, 7.500000000000000000 ) ) ;
#2838 = DIRECTION ( 'NONE',  ( 0.000000000000000000, 1.000000000000000000, 0.000000000000000000 ) ) ;
#2839 = CARTESIAN_POINT ( 'NONE',  ( -39.99999999999999289, 120.0000000000000284, 0.5000000000000000000 ) ) ;
#2840 = CARTESIAN_POINT ( 'NONE',  ( -15.29705854078139637, 0.8232575913729158756, -3.749818214850030626E-15 ) ) ;
#2841 = CARTESIAN_POINT ( 'NONE',  ( 22.00000000000002132, -100.0000000000000000, 7.500000000000000000 ) ) ;
#2842 = FACE_OUTER_BOUND ( 'NONE', #8879, .T. ) ;
#2843 = CARTESIAN_POINT ( 'NONE',  ( 35.00000000000000711, -25.00000000000000000, -7.500000000000000000 ) ) ;
#2844 = EDGE_CURVE ( 'NONE', #1473, #3310, #4071, .T. ) ;
#2845 = ORIENTED_EDGE ( 'NONE', *, *, #6497, .F. ) ;
#2846 = CARTESIAN_POINT ( 'NONE',  ( 5.138450363093609141, -111.7272727272695079, -0.006098328147151244397 ) ) ;
#2847 = ORIENTED_EDGE ( 'NONE', *, *, #11903, .T. ) ;
#2848 = CIRCLE ( 'NONE', #12484, 18.74900000001875355 ) ;
#2849 = EDGE_CURVE ( 'NONE', #2083, #6241, #9947, .T. ) ;
#2850 = ORIENTED_EDGE ( 'NONE', *, *, #7901, .T. ) ;
#2851 = DIRECTION ( 'NONE',  ( 0.000000000000000000, 1.000000000000000000, 0.000000000000000000 ) ) ;
#2852 = EDGE_CURVE ( 'NONE', #6776, #9459, #5190, .T. ) ;
#2853 = CARTESIAN_POINT ( 'NONE',  ( -10.00000000000000711, 97.99999999999994316, 0.5000000000000000000 ) ) ;
#2854 = DIRECTION ( 'NONE',  ( -2.797435172181481150E-17, 1.000000000000000000, -1.765856845898762549E-18 ) ) ;
#2855 = DIRECTION ( 'NONE',  ( 1.000000000000000000, 0.000000000000000000, 0.000000000000000000 ) ) ;
#2856 = DIRECTION ( 'NONE',  ( 1.000000000000000000, 0.000000000000000000, 0.000000000000000000 ) ) ;
#2857 = DIRECTION ( 'NONE',  ( 1.000000000000000000, 5.551115123125788224E-15, 0.000000000000000000 ) ) ;
#2858 = CIRCLE ( 'NONE', #2640, 23.64268088454700845 ) ;
#2859 = CARTESIAN_POINT ( 'NONE',  ( -30.68181818181819054, 131.1340442853780814, 2.499999999999999556 ) ) ;
#2860 = VERTEX_POINT ( 'NONE', #11014 ) ;
#2861 = B_SPLINE_CURVE_WITH_KNOTS ( 'NONE', 3,
 ( #8559, #3295, #11853, #11921, #10725, #7774, #8626, #5611, #300, #6660, #9683, #8835, #10857, #1267, #11786, #5534 ),
 .UNSPECIFIED., .F., .F.,
 ( 4, 2, 2, 2, 2, 2, 2, 4 ),
 ( 0.000000000000000000, 0.0009977135201011855421, 0.001496570280151775494, 0.001995427040202365446, 0.002494283800252954965, 0.002993140560303544917, 0.003491997320354134869, 0.003990854080404723954 ),
 .UNSPECIFIED. ) ;
#2862 = ORIENTED_EDGE ( 'NONE', *, *, #5099, .F. ) ;
#2863 = EDGE_CURVE ( 'NONE', #8344, #8462, #10568, .T. ) ;
#2864 = CARTESIAN_POINT ( 'NONE',  ( -0.9875499244693202172, -80.00464164737402939, 10.06307371418729701 ) ) ;
#2865 = ADVANCED_FACE ( 'NONE', ( #7866 ), #12502, .T. ) ;
#2866 = TOROIDAL_SURFACE ( 'NONE', #5317, 22.99999999999999289, 2.000000000000000000 ) ;
#2867 = ORIENTED_EDGE ( 'NONE', *, *, #3795, .T. ) ;
#2868 = CARTESIAN_POINT ( 'NONE',  ( 15.29705854078139460, -10.48808792804187284, -30.59411708156277854 ) ) ;
#2869 = CARTESIAN_POINT ( 'NONE',  ( 8.385254915620297567, 31.55439052270045508, -16.77050983124059158 ) ) ;
#2870 = EDGE_CURVE ( 'NONE', #6184, #9446, #11513, .T. ) ;
#2871 = CARTESIAN_POINT ( 'NONE',  ( 34.66997162884352690, 21.14050806081579736, -2.499999999999992895 ) ) ;
#2872 = CARTESIAN_POINT ( 'NONE',  ( -35.00000000000000000, -4.286263797015736496E-15, 4.000000000000000000 ) ) ;
#2873 = CARTESIAN_POINT ( 'NONE',  ( 8.470699010985018873, -93.30712875542430140, 0.4970230768060718840 ) ) ;
#2874 = CARTESIAN_POINT ( 'NONE',  ( 18.71826692230518674, -9.296782722394514309, -2.500000000000002665 ) ) ;
#2875 = AXIS2_PLACEMENT_3D ( 'NONE', #7353, #6191, #1836 ) ;
#2876 = EDGE_LOOP ( 'NONE', ( #2772, #12008, #8509, #8883 ) ) ;
#2877 = ORIENTED_EDGE ( 'NONE', *, *, #6865, .F. ) ;
#2878 = ORIENTED_EDGE ( 'NONE', *, *, #2223, .F. ) ;
#2879 = CARTESIAN_POINT ( 'NONE',  ( 15.18222645069203303, -16.04698886238941924, -4.000000000000000000 ) ) ;
#2880 = AXIS2_PLACEMENT_3D ( 'NONE', #777, #7419, #4977 ) ;
#2881 = ORIENTED_EDGE ( 'NONE', *, *, #5572, .T. ) ;
#2882 = CARTESIAN_POINT ( 'NONE',  ( -15.29705854078139105, -38.76242177807012723, -3.676584163678260711E-15 ) ) ;
#2883 = ORIENTED_EDGE ( 'NONE', *, *, #3693, .F. ) ;
#2884 = CARTESIAN_POINT ( 'NONE',  ( 8.385254915620292238, 90.00000000000000000, 8.679704431140118580E-16 ) ) ;
#2885 = FILL_AREA_STYLE ('',( #4706 ) ) ;
#2886 = AXIS2_PLACEMENT_3D ( 'NONE', #8842, #4857, #11240 ) ;
#2887 = B_SPLINE_CURVE_WITH_KNOTS ( 'NONE', 3,
 ( #13286, #12209, #10995, #3635, #2600, #1396, #6876, #1536, #5678, #4623, #3558, #13641, #4906, #10238, #12487, #1685 ),
 .UNSPECIFIED., .F., .F.,
 ( 4, 2, 2, 2, 2, 2, 2, 4 ),
 ( 1.969947839882000721E-07, 0.0003650593540107636178, 0.0007299217132375390368, 0.001094784072464314618, 0.001459646431691089983, 0.001824508790917865131, 0.002189371150144640930, 0.002919095868598201200 ),
 .UNSPECIFIED. ) ;
#2888 = EDGE_CURVE ( 'NONE', #3846, #7956, #11004, .T. ) ;
#2889 = CARTESIAN_POINT ( 'NONE',  ( -35.00000000000000000, -35.00000000000000000, -7.500000000000000000 ) ) ;
#2890 = CARTESIAN_POINT ( 'NONE',  ( 15.29705854078139105, 19.67281349139174296, 1.840275709580740132E-15 ) ) ;
#2891 = PLANE ( 'NONE',  #9545 ) ;
#2892 = CARTESIAN_POINT ( 'NONE',  ( -1.053348594425001616, -150.0300328178547318, -1.640268818953221963 ) ) ;
#2893 = DIRECTION ( 'NONE',  ( 0.9960067511297464593, -0.08927794634716622324, 3.401418580343279473E-17 ) ) ;
#2894 = ORIENTED_EDGE ( 'NONE', *, *, #8190, .F. ) ;
#2895 = CIRCLE ( 'NONE', #3105, 2.500000000000002220 ) ;
#2896 = ORIENTED_EDGE ( 'NONE', *, *, #701, .T. ) ;
#2897 = EDGE_LOOP ( 'NONE', ( #1158, #7841 ) ) ;
#2898 = DIRECTION ( 'NONE',  ( -0.3926913852462015631, -0.9196703082917374594, -2.775705599192072719E-16 ) ) ;
#2899 = DIRECTION ( 'NONE',  ( -2.797435172181481150E-17, 1.000000000000000000, -1.765856845898762549E-18 ) ) ;
#2900 = DIRECTION ( 'NONE',  ( 1.000000000000000000, 0.000000000000000000, 0.000000000000000000 ) ) ;
#2901 = LINE ( 'NONE', #806, #4356 ) ;
#2902 = CARTESIAN_POINT ( 'NONE',  ( -1.207220731154811100, -146.6502848478751275, 1.905708617823901108 ) ) ;
#2903 = CIRCLE ( 'NONE', #4912, 31.93204061526059334 ) ;
#2904 = CARTESIAN_POINT ( 'NONE',  ( -1.111302930823951263, -163.8787879467685116, -2.940232647904911012 ) ) ;
#2905 = CYLINDRICAL_SURFACE ( 'NONE', #9655, 8.385254915620294014 ) ;
#2906 = CARTESIAN_POINT ( 'NONE',  ( 0.000000000000000000, 71.01020514433645303, -0.5000000000000000000 ) ) ;
#2907 = DIRECTION ( 'NONE',  ( 0.000000000000000000, 0.000000000000000000, 1.000000000000000000 ) ) ;
#2908 = ADVANCED_FACE ( 'NONE', ( #4921 ), #12649, .F. ) ;
#2909 = AXIS2_PLACEMENT_3D ( 'NONE', #4225, #8240, #13749 ) ;
#2910 = DIRECTION ( 'NONE',  ( 1.000000000000000000, 0.000000000000000000, 0.000000000000000000 ) ) ;
#2911 = CARTESIAN_POINT ( 'NONE',  ( -8.385254915620297567, 31.55439052270045508, -1.138338632290247530E-15 ) ) ;
#2912 = CARTESIAN_POINT ( 'NONE',  ( 52.49999999999999289, 120.0000000000000142, -2.499999999999998668 ) ) ;
#2913 = ORIENTED_EDGE ( 'NONE', *, *, #8360, .F. ) ;
#2914 = DIRECTION ( 'NONE',  ( 0.9928035427100112553, 0.1197544386753605361, 9.637352644305958814E-17 ) ) ;
#2915 = CIRCLE ( 'NONE', #681, 1.999999999999998224 ) ;
#2916 = CARTESIAN_POINT ( 'NONE',  ( 4.560784247219194398, -95.36363636362298735, 0.7586904865634463979 ) ) ;
#2917 = CIRCLE ( 'NONE', #8503, 15.70031846811053455 ) ;
#2918 = EDGE_LOOP ( 'NONE', ( #10221, #4399 ) ) ;
#2919 = CIRCLE ( 'NONE', #2019, 5.000000000000000888 ) ;
#2920 = EDGE_LOOP ( 'NONE', ( #10332, #13431, #1314, #12772 ) ) ;
#2921 = DIRECTION ( 'NONE',  ( 0.6000000000000024203, -0.7999999999999982681, -0.000000000000000000 ) ) ;
#2922 = CARTESIAN_POINT ( 'NONE',  ( 35.00000000000000711, -25.00000000000000000, -4.000000000000000000 ) ) ;
#2923 = CARTESIAN_POINT ( 'NONE',  ( 4.588105241694418801, -161.0909090907375401, -0.3432044964428315192 ) ) ;
#2924 = EDGE_CURVE ( 'NONE', #10679, #7969, #9284, .T. ) ;
#2925 = TOROIDAL_SURFACE ( 'NONE', #6717, 17.49999999999999289, 5.000000000000000000 ) ;
#2926 = B_SPLINE_CURVE_WITH_KNOTS ( 'NONE', 3,
 ( #13027, #125, #7599, #1295 ),
 .UNSPECIFIED., .F., .F.,
 ( 4, 4 ),
 ( 0.000000000000000000, 1.000000000000000000 ),
 .UNSPECIFIED. ) ;
#2927 = CARTESIAN_POINT ( 'NONE',  ( 25.00000000000001776, -99.15310334213020838, 3.061571689641656246E-15 ) ) ;
#2928 = CARTESIAN_POINT ( 'NONE',  ( 12.99553232110413958, 48.77386654458962312, 3.182987412051232168E-15 ) ) ;
#2929 = EDGE_CURVE ( 'NONE', #5523, #13483, #421, .T. ) ;
#2930 = ADVANCED_FACE ( 'NONE', ( #1062 ), #7429, .T. ) ;
#2931 = AXIS2_PLACEMENT_3D ( 'NONE', #7129, #11405, #6089 ) ;
#2932 = CARTESIAN_POINT ( 'NONE',  ( -10.69381717166375623, 16.13466892210585613, -1.366597928139322991E-15 ) ) ;
#2933 = VECTOR ( 'NONE', #11026, 1000.000000000000000 ) ;
#2934 = CARTESIAN_POINT ( 'NONE',  ( -4.658064847839354705, 90.49194140877688142, 1.819915145876240370 ) ) ;
#2935 = EDGE_CURVE ( 'NONE', #10108, #10478, #5401, .T. ) ;
#2936 = EDGE_CURVE ( 'NONE', #13011, #11197, #6215, .T. ) ;
#2937 = EDGE_LOOP ( 'NONE', ( #11427, #7187, #12929, #652, #2231 ) ) ;
#2938 = VECTOR ( 'NONE', #9092, 1000.000000000000000 ) ;
#2939 = CARTESIAN_POINT ( 'NONE',  ( -5.035065420445773654, -83.15251865640357209, 8.244702687588977952 ) ) ;
#2940 = ORIENTED_EDGE ( 'NONE', *, *, #1122, .F. ) ;
#2941 = ORIENTED_EDGE ( 'NONE', *, *, #984, .T. ) ;
#2942 = CARTESIAN_POINT ( 'NONE',  ( -8.385254915620292238, -22.36966495935058319, -2.016610837207367011E-15 ) ) ;
#2943 = B_SPLINE_CURVE_WITH_KNOTS ( 'NONE', 3,
 ( #13250, #1650, #10269, #3674, #3522, #7959, #6979, #5866, #6761, #10138, #547, #11323, #2706, #611, #12094, #4809 ),
 .UNSPECIFIED., .F., .F.,
 ( 4, 2, 2, 2, 2, 2, 2, 4 ),
 ( 0.000000000000000000, 0.0003997740159331187953, 0.0007995480318662375905, 0.001599096063732475181, 0.001998870079665579936, 0.002398644095598684474, 0.002798418111531789012, 0.003198192127464893550 ),
 .UNSPECIFIED. ) ;
#2944 = DIRECTION ( 'NONE',  ( -0.3926913852462015631, -0.9196703082917374594, -2.775705599192072719E-16 ) ) ;
#2945 = CARTESIAN_POINT ( 'NONE',  ( 34.31344059123750867, 108.0182175921209051, 1.328634118392873598 ) ) ;
#2946 = CARTESIAN_POINT ( 'NONE',  ( -15.29705854078138749, -1.063309978032445979, -30.59411708156277854 ) ) ;
#2947 = CARTESIAN_POINT ( 'NONE',  ( 2.958050194273104783, -139.3718435583852227, -0.4183503205596436625 ) ) ;
#2948 = CARTESIAN_POINT ( 'NONE',  ( 8.385254915620290461, 79.99058638175036151, 8.868043070384787486E-16 ) ) ;
#2949 = VERTEX_POINT ( 'NONE', #6146 ) ;
#2950 = EDGE_CURVE ( 'NONE', #4148, #5091, #12833, .T. ) ;
#2951 = AXIS2_PLACEMENT_3D ( 'NONE', #4288, #8568, #3234 ) ;
#2952 = EDGE_LOOP ( 'NONE', ( #2668, #7333, #9668, #861 ) ) ;
#2953 = VERTEX_POINT ( 'NONE', #4091 ) ;
#2954 = ORIENTED_EDGE ( 'NONE', *, *, #12971, .F. ) ;
#2955 = CARTESIAN_POINT ( 'NONE',  ( -35.00000000000000000, -4.286263797015736496E-15, 7.500000000000000000 ) ) ;
#2956 = VERTEX_POINT ( 'NONE', #7318 ) ;
#2957 = CARTESIAN_POINT ( 'NONE',  ( 12.97449437267217753, -39.59556244224027211, 1.645560741966129631E-15 ) ) ;
#2958 = VERTEX_POINT ( 'NONE', #3109 ) ;
#2959 = CARTESIAN_POINT ( 'NONE',  ( 15.29705854078138927, 90.00000000000000000, 1.714422261702872766E-15 ) ) ;
#2960 = AXIS2_PLACEMENT_3D ( 'NONE', #7185, #1856, #6274 ) ;
#2961 = FACE_OUTER_BOUND ( 'NONE', #10260, .T. ) ;
#2962 = CARTESIAN_POINT ( 'NONE',  ( -5.912741552701379355, -73.45454545179654815, -18.82838426746663174 ) ) ;
#2963 = DIRECTION ( 'NONE',  ( -6.158143864569485777E-17, -2.736152283717910599E-16, 1.000000000000000000 ) ) ;
#2964 = B_SPLINE_CURVE_WITH_KNOTS ( 'NONE', 3,
 ( #1496, #5776, #8434, #13738, #7171, #5075, #11922, #11854, #10859, #229 ),
 .UNSPECIFIED., .F., .F.,
 ( 4, 3, 3, 4 ),
 ( 0.000000000000000000, 0.0007726433382168586489, 0.001886030654550297121, 0.002999417971186700387 ),
 .UNSPECIFIED. ) ;
#2965 = CARTESIAN_POINT ( 'NONE',  ( 5.478016874438395689, -117.3626624613967806, 1.011505465123966552 ) ) ;
#2966 = DIRECTION ( 'NONE',  ( 6.158143864569485777E-17, 2.736152283717910599E-16, -1.000000000000000000 ) ) ;
#2967 = EDGE_CURVE ( 'NONE', #6908, #6441, #13285, .T. ) ;
#2968 = EDGE_LOOP ( 'NONE', ( #11431, #4933, #5782, #12981 ) ) ;
#2969 = VERTEX_POINT ( 'NONE', #1995 ) ;
#2970 = ORIENTED_EDGE ( 'NONE', *, *, #7135, .T. ) ;
#2971 = DIRECTION ( 'NONE',  ( -1.000000000000000000, 0.000000000000000000, 0.000000000000000000 ) ) ;
#2972 = DIRECTION ( 'NONE',  ( 0.9960067511297463483, -0.08927794634716620936, 4.626175998653454121E-17 ) ) ;
#2973 = CARTESIAN_POINT ( 'NONE',  ( 5.059189827636713765, -83.15590270883112112, -8.262539084012589186 ) ) ;
#2974 = CARTESIAN_POINT ( 'NONE',  ( -0.5850150888136983474, -160.9696969704900482, 1.917718896956037700 ) ) ;
#2975 = DIRECTION ( 'NONE',  ( 0.000000000000000000, 0.000000000000000000, 1.000000000000000000 ) ) ;
#2976 = DIRECTION ( 'NONE',  ( -1.000000000000000000, 0.000000000000000000, 0.000000000000000000 ) ) ;
#2977 = DIRECTION ( 'NONE',  ( 1.000000000000000000, 0.000000000000000000, 0.000000000000000000 ) ) ;
#2978 = CARTESIAN_POINT ( 'NONE',  ( -15.29705854078139282, 90.00000000000000000, -1.589271161308885878E-16 ) ) ;
#2979 = ORIENTED_EDGE ( 'NONE', *, *, #3269, .F. ) ;
#2980 = AXIS2_PLACEMENT_3D ( 'NONE', #7985, #5731, #4680 ) ;
#2981 = DIRECTION ( 'NONE',  ( 0.000000000000000000, 0.000000000000000000, 1.000000000000000000 ) ) ;
#2982 = CARTESIAN_POINT ( 'NONE',  ( 12.66071438417660922, -140.5584415584655460, 5.506376209459975080 ) ) ;
#2983 = AXIS2_PLACEMENT_3D ( 'NONE', #3063, #965, #13827 ) ;
#2984 = VERTEX_POINT ( 'NONE', #2912 ) ;
#2985 = EDGE_CURVE ( 'NONE', #3080, #2423, #12601, .T. ) ;
#2986 = ORIENTED_EDGE ( 'NONE', *, *, #7531, .F. ) ;
#2987 = CARTESIAN_POINT ( 'NONE',  ( -4.330127018922201643, 91.72908881866754882, -2.499999999999993783 ) ) ;
#2988 = CARTESIAN_POINT ( 'NONE',  ( 25.00000000000000355, 120.0000000000000142, -0.5000000000000000000 ) ) ;
#2989 = CARTESIAN_POINT ( 'NONE',  ( 14.10210168181666468, -21.78333407367942698, -6.931746760319976275 ) ) ;
#2990 = AXIS2_PLACEMENT_3D ( 'NONE', #4490, #1331, #13298 ) ;
#2991 = CARTESIAN_POINT ( 'NONE',  ( -3.361332843921210234, -147.1038961038632067, -14.17852599539660297 ) ) ;
#2992 = CARTESIAN_POINT ( 'NONE',  ( -10.00000000000000711, 139.9999999999999716, -0.5000000000000000000 ) ) ;
#2993 = CARTESIAN_POINT ( 'NONE',  ( 15.29705854078139105, -36.87585420866476227, 3.746698755667522411E-15 ) ) ;
#2994 = CARTESIAN_POINT ( 'NONE',  ( -4.338055960494663132, 91.73205429892865936, 2.486400748338238653 ) ) ;
#2995 = ORIENTED_EDGE ( 'NONE', *, *, #12917, .F. ) ;
#2996 = VECTOR ( 'NONE', #4665, 1000.000000000000000 ) ;
#2997 = EDGE_CURVE ( 'NONE', #1745, #13042, #1170, .T. ) ;
#2998 = CARTESIAN_POINT ( 'NONE',  ( -8.844020276311006512, -89.05663101222295097, 1.691421750721286088 ) ) ;
#2999 = EDGE_CURVE ( 'NONE', #8545, #3001, #11535, .T. ) ;
#3000 = CIRCLE ( 'NONE', #9053, 4.999999999999998224 ) ;
#3001 = VERTEX_POINT ( 'NONE', #5146 ) ;
#3002 = EDGE_CURVE ( 'NONE', #6314, #8647, #2060, .T. ) ;
#3003 = CARTESIAN_POINT ( 'NONE',  ( -35.00000000000012079, 91.25000000000045475, 7.500000000000000000 ) ) ;
#3004 = CARTESIAN_POINT ( 'NONE',  ( -60.00000000000001421, -4.286263797015736496E-15, -4.000000000000000000 ) ) ;
#3005 = CARTESIAN_POINT ( 'NONE',  ( 34.98870950856983342, 106.6817206552402268, 2.472621650539469584 ) ) ;
#3006 = CARTESIAN_POINT ( 'NONE',  ( -15.29705854078138927, 57.37192529142945574, -1.013106070382630377E-16 ) ) ;
#3007 = CARTESIAN_POINT ( 'NONE',  ( 2.997639754412456892, -137.4006169092532161, -1.171341992379282715 ) ) ;
#3008 = CARTESIAN_POINT ( 'NONE',  ( 48.00000000000000000, 120.0000000000000142, -0.5000000000000000000 ) ) ;
#3009 = ORIENTED_EDGE ( 'NONE', *, *, #352, .F. ) ;
#3010 = VERTEX_POINT ( 'NONE', #9437 ) ;
#3011 = ORIENTED_EDGE ( 'NONE', *, *, #517, .F. ) ;
#3012 = CYLINDRICAL_SURFACE ( 'NONE', #8089, 15.29705854078139105 ) ;
#3013 = ORIENTED_EDGE ( 'NONE', *, *, #10866, .T. ) ;
#3014 = VECTOR ( 'NONE', #12905, 1000.000000000000000 ) ;
#3015 = EDGE_CURVE ( 'NONE', #3108, #11568, #11601, .T. ) ;
#3016 = CIRCLE ( 'NONE', #10832, 79.99999999999997158 ) ;
#3017 = VERTEX_POINT ( 'NONE', #9501 ) ;
#3018 = CARTESIAN_POINT ( 'NONE',  ( -2.504624958784990426E-13, 92.00000000000000000, -4.500000000000000888 ) ) ;
#3019 = ORIENTED_EDGE ( 'NONE', *, *, #9530, .F. ) ;
#3020 = CARTESIAN_POINT ( 'NONE',  ( -32.95454545454546746, 135.5876619995293311, 7.500000000000000000 ) ) ;
#3021 = AXIS2_PLACEMENT_3D ( 'NONE', #7463, #1165, #51 ) ;
#3022 = EDGE_LOOP ( 'NONE', ( #7971, #2587, #11100, #11127 ) ) ;
#3023 = EDGE_CURVE ( 'NONE', #8382, #5087, #4161, .T. ) ;
#3024 = CARTESIAN_POINT ( 'NONE',  ( -10.00000000000000000, 90.00000000000000000, 0.5000000000000000000 ) ) ;
#3025 = EDGE_CURVE ( 'NONE', #4480, #6588, #54, .T. ) ;
#3026 = CARTESIAN_POINT ( 'NONE',  ( -8.597717047221227205, -85.78354978359179484, 6.129448613111333266 ) ) ;
#3027 = FACE_BOUND ( 'NONE', #9859, .T. ) ;
#3028 = CARTESIAN_POINT ( 'NONE',  ( -15.66041902283167175, -22.75225252538439236, 1.300500990791220168 ) ) ;
#3029 = DIRECTION ( 'NONE',  ( 0.9928035427100113663, 0.1197544386753605777, 9.252351997306908241E-17 ) ) ;
#3030 = CARTESIAN_POINT ( 'NONE',  ( -2.416244575755594148, -133.5561241431034887, 2.746148655430789454 ) ) ;
#3031 = CARTESIAN_POINT ( 'NONE',  ( 34.99999999999958789, 1.091249486606660213E-13, 2.500000000000000000 ) ) ;
#3032 = TOROIDAL_SURFACE ( 'NONE', #13591, 16.99999999999998934, 2.000000000000000000 ) ;
#3033 = EDGE_LOOP ( 'NONE', ( #3076, #9189, #13236, #8479 ) ) ;
#3034 = EDGE_LOOP ( 'NONE', ( #11101, #4938, #7770, #12252, #1758, #516 ) ) ;
#3035 = MECHANICAL_DESIGN_GEOMETRIC_PRESENTATION_REPRESENTATION (  '', ( #1461 ), #6605 ) ;
#3036 = ORIENTED_EDGE ( 'NONE', *, *, #2936, .F. ) ;
#3037 = CARTESIAN_POINT ( 'NONE',  ( -0.3297608091563175581, -142.6355133186271757, -2.624337192179055478 ) ) ;
#3038 = LINE ( 'NONE', #4080, #12312 ) ;
#3039 = CIRCLE ( 'NONE', #4839, 2.500000000000002220 ) ;
#3040 = DIRECTION ( 'NONE',  ( -0.000000000000000000, -0.000000000000000000, -1.000000000000000000 ) ) ;
#3041 = CARTESIAN_POINT ( 'NONE',  ( 6.326212770466429269, -95.26718119391159689, 5.262869407572682512 ) ) ;
#3042 = ADVANCED_FACE ( 'NONE', ( #7835 ), #7877, .F. ) ;
#3043 = CARTESIAN_POINT ( 'NONE',  ( 8.385254915620290461, 62.45333659073424570, -16.77050983124057737 ) ) ;
#3044 = LINE ( 'NONE', #10672, #8500 ) ;
#3045 = CIRCLE ( 'NONE', #9315, 2.500000000000002220 ) ;
#3046 = CARTESIAN_POINT ( 'NONE',  ( 58.70736094381068426, -9.392073098158826738, -2.500000000000000000 ) ) ;
#3047 = CARTESIAN_POINT ( 'NONE',  ( 10.00000000000000711, 139.9999999999999716, -2.500000000000000000 ) ) ;
#3048 = CARTESIAN_POINT ( 'NONE',  ( 15.29705854078139282, -1.063309978032472403, 1.873561326908939435E-15 ) ) ;
#3049 = AXIS2_PLACEMENT_3D ( 'NONE', #1748, #10373, #9184 ) ;
#3050 = EDGE_LOOP ( 'NONE', ( #13784, #4749, #5332, #9024 ) ) ;
#3051 = CARTESIAN_POINT ( 'NONE',  ( -35.00000000000000000, -4.286263797015736496E-15, -4.000000000000000000 ) ) ;
#3052 = EDGE_LOOP ( 'NONE', ( #661, #11638, #2374, #7252, #7405, #6128, #12374, #9806, #2970, #716, #2728, #8460, #6000 ) ) ;
#3053 = DIRECTION ( 'NONE',  ( 0.000000000000000000, 0.000000000000000000, 1.000000000000000000 ) ) ;
#3054 = ORIENTED_EDGE ( 'NONE', *, *, #7896, .T. ) ;
#3055 = LINE ( 'NONE', #8651, #1683 ) ;
#3056 = MANIFOLD_SOLID_BREP ( 'Fillet1', #2005 ) ;
#3057 = DIRECTION ( 'NONE',  ( -2.797435172181481150E-17, 1.000000000000000000, -1.765856845898762549E-18 ) ) ;
#3058 = DIRECTION ( 'NONE',  ( 0.000000000000000000, 1.000000000000000000, 0.000000000000000000 ) ) ;
#3059 = CARTESIAN_POINT ( 'NONE',  ( 0.003226301100676102433, -100.2727272727208856, 4.613888802083836893 ) ) ;
#3060 = B_SPLINE_CURVE_WITH_KNOTS ( 'NONE', 3,
 ( #13331, #3681, #12249, #6905 ),
 .UNSPECIFIED., .F., .F.,
 ( 4, 4 ),
 ( 0.000000000000000000, 1.000000000000000000 ),
 .UNSPECIFIED. ) ;
#3061 = CARTESIAN_POINT ( 'NONE',  ( 58.40844909094411719, 10.11407490371516182, 2.500000000000004441 ) ) ;
#3062 = CARTESIAN_POINT ( 'NONE',  ( 8.385254915620292238, -22.36966495935058319, 2.053795118489800004E-15 ) ) ;
#3063 = CARTESIAN_POINT ( 'NONE',  ( -35.00000000000000000, -4.286263797015736496E-15, 8.499999999999998224 ) ) ;
#3064 = DIRECTION ( 'NONE',  ( 1.000000000000000000, 0.000000000000000000, 0.000000000000000000 ) ) ;
#3065 = AXIS2_PLACEMENT_3D ( 'NONE', #6709, #9799, #7545 ) ;
#3066 = ORIENTED_EDGE ( 'NONE', *, *, #3373, .T. ) ;
#3067 = ORIENTED_EDGE ( 'NONE', *, *, #301, .T. ) ;
#3068 = CARTESIAN_POINT ( 'NONE',  ( -12.99579180576516890, -11.31471392308272605, -3.182109625360474349E-15 ) ) ;
#3069 = DIRECTION ( 'NONE',  ( -6.158143864569485777E-17, -2.736152283717910599E-16, 1.000000000000000000 ) ) ;
#3070 = TOROIDAL_SURFACE ( 'NONE', #6646, 22.99999999999999289, 2.000000000000000000 ) ;
#3071 = CARTESIAN_POINT ( 'NONE',  ( -15.29705854078139460, 55.48535772202409078, -2.069307775394917278E-15 ) ) ;
#3072 = CARTESIAN_POINT ( 'NONE',  ( 15.29705854078139460, -1.063309978032445091, -30.59411708156277854 ) ) ;
#3073 = DIRECTION ( 'NONE',  ( -2.797435172181481150E-17, 1.000000000000000000, -1.765856845898762549E-18 ) ) ;
#3074 = ADVANCED_FACE ( 'NONE', ( #4989 ), #8231, .T. ) ;
#3075 = CARTESIAN_POINT ( 'NONE',  ( -15.29705854078139282, 47.94714734142005597, -3.833032258170527700E-15 ) ) ;
#3076 = ORIENTED_EDGE ( 'NONE', *, *, #8071, .F. ) ;
#3077 = ORIENTED_EDGE ( 'NONE', *, *, #3701, .T. ) ;
#3078 = ORIENTED_EDGE ( 'NONE', *, *, #4460, .T. ) ;
#3079 = CARTESIAN_POINT ( 'NONE',  ( -2.517691654963332357E-15, 90.00000000000000000, -1.589271161308885878E-16 ) ) ;
#3080 = VERTEX_POINT ( 'NONE', #3743 ) ;
#3081 = DIRECTION ( 'NONE',  ( 1.000000000000000000, 0.000000000000000000, 0.000000000000000000 ) ) ;
#3082 = VERTEX_POINT ( 'NONE', #12307 ) ;
#3083 = FACE_OUTER_BOUND ( 'NONE', #1608, .T. ) ;
#3084 = CARTESIAN_POINT ( 'NONE',  ( -6.213657885899291244, -97.41991341993369247, -5.968417174478657827 ) ) ;
#3085 = DIRECTION ( 'NONE',  ( 0.000000000000000000, 0.000000000000000000, 1.000000000000000000 ) ) ;
#3086 = CARTESIAN_POINT ( 'NONE',  ( 34.99999999999958789, 1.091249486606660213E-13, 2.500000000000000000 ) ) ;
#3087 = CARTESIAN_POINT ( 'NONE',  ( -0.6173387890061908800, -69.99999999999998579, 4.961742921553712549 ) ) ;
#3088 = CARTESIAN_POINT ( 'NONE',  ( 10.11726280447958182, 5.576682675210010487, -2.499999999999999112 ) ) ;
#3089 = CARTESIAN_POINT ( 'NONE',  ( 8.385254915620292238, 69.25350232273815720, 9.631531405059307235E-16 ) ) ;
#3090 = ADVANCED_FACE ( 'NONE', ( #8027 ), #12907, .T. ) ;
#3091 = CARTESIAN_POINT ( 'NONE',  ( 5.650019569485428050, -113.2088557674236000, -2.224334737347880786 ) ) ;
#3092 = CARTESIAN_POINT ( 'NONE',  ( 35.00000000000000000, 4.286263797015736496E-15, -4.000000000000000000 ) ) ;
#3093 = EDGE_CURVE ( 'NONE', #7898, #11376, #12141, .T. ) ;
#3094 = VERTEX_POINT ( 'NONE', #8893 ) ;
#3095 = ORIENTED_EDGE ( 'NONE', *, *, #540, .T. ) ;
#3096 = EDGE_CURVE ( 'NONE', #9459, #12157, #1844, .T. ) ;
#3097 = EDGE_CURVE ( 'NONE', #2556, #9444, #12984, .T. ) ;
#3098 = CIRCLE ( 'NONE', #199, 25.00000000000000355 ) ;
#3099 = DIRECTION ( 'NONE',  ( 0.8907235428302464619, 0.4545454545454548079, 0.000000000000000000 ) ) ;
#3100 = LINE ( 'NONE', #6206, #586 ) ;
#3101 = CARTESIAN_POINT ( 'NONE',  ( 7.692922818056756817, -86.09451208659135091, -5.376924148044465390 ) ) ;
#3102 = CARTESIAN_POINT ( 'NONE',  ( 0.000000000000000000, 71.01020514433645303, 2.499999999999999556 ) ) ;
#3103 = DIRECTION ( 'NONE',  ( -0.000000000000000000, 1.000000000000000000, -0.000000000000000000 ) ) ;
#3104 = LINE ( 'NONE', #7246, #822 ) ;
#3105 = AXIS2_PLACEMENT_3D ( 'NONE', #567, #7912, #6713 ) ;
#3106 = DIRECTION ( 'NONE',  ( -1.000000000000000000, 0.000000000000000000, 0.000000000000000000 ) ) ;
#3107 = CARTESIAN_POINT ( 'NONE',  ( 10.69346802281034670, 30.74929022373126841, 2.619144277183853555E-15 ) ) ;
#3108 = VERTEX_POINT ( 'NONE', #8752 ) ;
#3109 = CARTESIAN_POINT ( 'NONE',  ( 15.29705854078139282, -38.76242177807012723, 1.940132561565339224E-15 ) ) ;
#3110 = EDGE_CURVE ( 'NONE', #1805, #3210, #5856, .T. ) ;
#3111 = FACE_BOUND ( 'NONE', #12341, .T. ) ;
#3112 = CARTESIAN_POINT ( 'NONE',  ( -12.09338464843076189, -169.0000000000000568, 0.006909782850911748778 ) ) ;
#3113 = VERTEX_POINT ( 'NONE', #3416 ) ;
#3114 = CARTESIAN_POINT ( 'NONE',  ( -2.517691654963332357E-15, 90.00000000000000000, -1.589271161308885878E-16 ) ) ;
#3115 = ORIENTED_EDGE ( 'NONE', *, *, #12623, .F. ) ;
#3116 = CARTESIAN_POINT ( 'NONE',  ( 12.99579180576516890, -11.31471392308272605, 0.000000000000000000 ) ) ;
#3117 = FACE_OUTER_BOUND ( 'NONE', #10053, .T. ) ;
#3118 = CARTESIAN_POINT ( 'NONE',  ( 1.174765158563475076, -79.03030302990762834, 10.44010582255705444 ) ) ;
#3119 = CARTESIAN_POINT ( 'NONE',  ( -2.886819890957894152, -105.1818181818214839, 3.599275682873828153 ) ) ;
#3120 = CARTESIAN_POINT ( 'NONE',  ( 35.00000000000009237, 91.25000000000046896, 7.500000000000000000 ) ) ;
#3121 = CARTESIAN_POINT ( 'NONE',  ( 8.385254915620294014, 50.40394642271930792, 2.053795118489800793E-15 ) ) ;
#3122 = CARTESIAN_POINT ( 'NONE',  ( 15.29705854078139105, -36.87585420866476227, 1.940132561565339224E-15 ) ) ;
#3123 = CARTESIAN_POINT ( 'NONE',  ( -12.99579180576516535, 16.95961992694555676, -1.651422005635246569E-15 ) ) ;
#3124 = AXIS2_PLACEMENT_3D ( 'NONE', #13005, #2185, #2466 ) ;
#3125 = ADVANCED_FACE ( 'NONE', ( #4266 ), #4196, .T. ) ;
#3126 = AXIS2_PLACEMENT_3D ( 'NONE', #13264, #2639, #8112 ) ;
#3127 = VERTEX_POINT ( 'NONE', #6448 ) ;
#3128 = VECTOR ( 'NONE', #3557, 1000.000000000000000 ) ;
#3129 = ORIENTED_EDGE ( 'NONE', *, *, #1642, .F. ) ;
#3130 = CARTESIAN_POINT ( 'NONE',  ( -8.385254915620292238, 53.02855864072483882, -9.364084330386787485E-17 ) ) ;
#3131 = DIRECTION ( 'NONE',  ( -0.9462100554738961389, -0.3235529800822216639, -1.445602896645893329E-16 ) ) ;
#3132 = AXIS2_PLACEMENT_3D ( 'NONE', #5561, #4511, #6691 ) ;
#3133 = AXIS2_PLACEMENT_3D ( 'NONE', #1126, #2364, #5382 ) ;
#3134 = CARTESIAN_POINT ( 'NONE',  ( 35.00000000000000000, 4.286263797015736496E-15, 7.500000000000000000 ) ) ;
#3135 = DIRECTION ( 'NONE',  ( 1.000000000000000000, 2.797435172181480534E-17, -0.000000000000000000 ) ) ;
#3136 = CYLINDRICAL_SURFACE ( 'NONE', #9483, 8.385254915620292238 ) ;
#3137 = DIRECTION ( 'NONE',  ( 1.000000000000000000, -0.000000000000000000, 0.000000000000000000 ) ) ;
#3138 = ORIENTED_EDGE ( 'NONE', *, *, #3565, .F. ) ;
#3139 = CIRCLE ( 'NONE', #7183, 2.000000000000003109 ) ;
#3140 = AXIS2_PLACEMENT_3D ( 'NONE', #9537, #6699, #12766 ) ;
#3141 = EDGE_CURVE ( 'NONE', #30, #11958, #4961, .T. ) ;
#3142 = CARTESIAN_POINT ( 'NONE',  ( -15.29705854078139105, -10.48808792804187284, 1.852046186812095429E-17 ) ) ;
#3143 = CARTESIAN_POINT ( 'NONE',  ( 15.29705854078138749, 76.22148119144830503, 1.740418857596141236E-15 ) ) ;
#3144 = ORIENTED_EDGE ( 'NONE', *, *, #10130, .T. ) ;
#3145 = FACE_OUTER_BOUND ( 'NONE', #7216, .T. ) ;
#3146 = AXIS2_PLACEMENT_3D ( 'NONE', #7655, #7583, #2261 ) ;
#3147 = APPLICATION_CONTEXT ( 'automotive_design' ) ;
#3148 = DIRECTION ( 'NONE',  ( -0.8907235428302473501, 0.4545454545454531425, 0.000000000000000000 ) ) ;
#3149 = DIRECTION ( 'NONE',  ( 1.000000000000000000, 1.224646799147353207E-16, 0.000000000000000000 ) ) ;
#3150 = AXIS2_PLACEMENT_3D ( 'NONE', #12021, #5307, #9659 ) ;
#3151 = CARTESIAN_POINT ( 'NONE',  ( -24.99999999999999289, -99.52837026979777590, 3.391106264173251450 ) ) ;
#3152 = DIRECTION ( 'NONE',  ( -1.224646799147353207E-16, 1.000000000000000000, -0.000000000000000000 ) ) ;
#3153 = CIRCLE ( 'NONE', #1810, 2.500000000000002220 ) ;
#3154 = CARTESIAN_POINT ( 'NONE',  ( -0.8598734018918594568, -151.0707854172325426, -1.652135397942386064 ) ) ;
#3155 = CARTESIAN_POINT ( 'NONE',  ( 25.00000000000001776, -100.0000000000000000, -7.500000000000000000 ) ) ;
#3156 = VERTEX_POINT ( 'NONE', #2164 ) ;
#3157 = ORIENTED_EDGE ( 'NONE', *, *, #8437, .T. ) ;
#3158 = ORIENTED_EDGE ( 'NONE', *, *, #6531, .F. ) ;
#3159 = AXIS2_PLACEMENT_3D ( 'NONE', #593, #2540, #4711 ) ;
#3160 = AXIS2_PLACEMENT_3D ( 'NONE', #3102, #2975, #2055 ) ;
#3161 = EDGE_CURVE ( 'NONE', #1460, #10921, #2254, .T. ) ;
#3162 = CYLINDRICAL_SURFACE ( 'NONE', #12756, 14.99999999999998934 ) ;
#3163 = EDGE_CURVE ( 'NONE', #2525, #9172, #4260, .T. ) ;
#3164 = ORIENTED_EDGE ( 'NONE', *, *, #3334, .F. ) ;
#3165 = CARTESIAN_POINT ( 'NONE',  ( 34.99999999999958789, 1.104930248025249758E-13, -2.499999999999999112 ) ) ;
#3166 = CARTESIAN_POINT ( 'NONE',  ( 7.846342596345671438, -93.17560321804917578, 3.276283083350423730 ) ) ;
#3167 = CARTESIAN_POINT ( 'NONE',  ( -15.29705854078138927, -8.601520358636511432, -30.59411708156278564 ) ) ;
#3168 = CYLINDRICAL_SURFACE ( 'NONE', #2731, 8.385254915620292238 ) ;
#3169 = CARTESIAN_POINT ( 'NONE',  ( -2.008006351130390499, -80.00378950643924725, -9.910921267331605833 ) ) ;
#3170 = ADVANCED_FACE ( 'NONE', ( #7630 ), #9607, .T. ) ;
#3171 = CARTESIAN_POINT ( 'NONE',  ( -8.385254915620290461, 22.12961257269105531, -16.77050983124058803 ) ) ;
#3172 = EDGE_CURVE ( 'NONE', #2573, #6716, #9218, .T. ) ;
#3173 = CARTESIAN_POINT ( 'NONE',  ( 0.2899689842974736975, -80.99999999999971578, -10.01379011345939851 ) ) ;
#3174 = DIRECTION ( 'NONE',  ( 0.000000000000000000, 0.000000000000000000, 1.000000000000000000 ) ) ;
#3175 = CARTESIAN_POINT ( 'NONE',  ( -12.99553232110414491, 29.92431064457076673, 25.99106464220827917 ) ) ;
#3176 = VERTEX_POINT ( 'NONE', #7763 ) ;
#3177 = LINE ( 'NONE', #1087, #6088 ) ;
#3178 = CARTESIAN_POINT ( 'NONE',  ( 15.29705854078139460, 74.33491362204296138, -30.59411708156277854 ) ) ;
#3179 = ORIENTED_EDGE ( 'NONE', *, *, #8308, .F. ) ;
#3180 = CARTESIAN_POINT ( 'NONE',  ( 47.69307742500824787, -16.90904448151677286, 2.499999999999996003 ) ) ;
#3181 = ORIENTED_EDGE ( 'NONE', *, *, #9673, .T. ) ;
#3182 = EDGE_CURVE ( 'NONE', #6151, #6555, #10711, .T. ) ;
#3183 = FACE_OUTER_BOUND ( 'NONE', #10497, .T. ) ;
#3184 = EDGE_CURVE ( 'NONE', #8450, #8647, #11227, .T. ) ;
#3185 = EDGE_LOOP ( 'NONE', ( #1740, #3875, #8359, #13169 ) ) ;
#3186 = DIRECTION ( 'NONE',  ( 1.000000000000000000, 0.000000000000000000, 0.000000000000000000 ) ) ;
#3187 = DIRECTION ( 'NONE',  ( -0.000000000000000000, -0.000000000000000000, -1.000000000000000000 ) ) ;
#3188 = CARTESIAN_POINT ( 'NONE',  ( 8.355983819232738696, -73.45454545667848834, 17.50953411836414730 ) ) ;
#3189 = EDGE_CURVE ( 'NONE', #12042, #8931, #4052, .T. ) ;
#3190 = CARTESIAN_POINT ( 'NONE',  ( 4.980291965142508381, -118.2727272727225056, 1.265069668247140955 ) ) ;
#3191 = EDGE_CURVE ( 'NONE', #1947, #8894, #12921, .T. ) ;
#3192 = CARTESIAN_POINT ( 'NONE',  ( -12.99553232110413958, 11.07475474455194053, -3.208141528222677273E-15 ) ) ;
#3193 = DIRECTION ( 'NONE',  ( 1.000000000000000000, 0.000000000000000000, 0.000000000000000000 ) ) ;
#3194 = DIRECTION ( 'NONE',  ( -1.000000000000000000, 0.000000000000000000, 0.000000000000000000 ) ) ;
#3195 = AXIS2_PLACEMENT_3D ( 'NONE', #11966, #11898, #3405 ) ;
#3196 = DIRECTION ( 'NONE',  ( 0.000000000000000000, 0.000000000000000000, 1.000000000000000000 ) ) ;
#3197 = ORIENTED_EDGE ( 'NONE', *, *, #3710, .T. ) ;
#3198 = CIRCLE ( 'NONE', #6134, 9.000000000009000800 ) ;
#3199 = CARTESIAN_POINT ( 'NONE',  ( 0.000000000000000000, 0.000000000000000000, 0.000000000000000000 ) ) ;
#3200 = EDGE_LOOP ( 'NONE', ( #7220, #6516, #4931, #8490 ) ) ;
#3201 = FACE_OUTER_BOUND ( 'NONE', #8209, .T. ) ;
#3202 = CARTESIAN_POINT ( 'NONE',  ( 0.000000000000000000, -20.00000000000000000, 20.00000000000000000 ) ) ;
#3203 = EDGE_CURVE ( 'NONE', #9139, #2025, #7186, .T. ) ;
#3204 = LINE ( 'NONE', #1307, #2375 ) ;
#3205 = CARTESIAN_POINT ( 'NONE',  ( -6.266477149339306330, -76.69310177716063492, -7.966230677900265178 ) ) ;
#3206 = CYLINDRICAL_SURFACE ( 'NONE', #3870, 67.49999999999997158 ) ;
#3207 = DIRECTION ( 'NONE',  ( -0.000000000000000000, -0.000000000000000000, -1.000000000000000000 ) ) ;
#3208 = CIRCLE ( 'NONE', #2311, 18.74900000001875000 ) ;
#3209 = VERTEX_POINT ( 'NONE', #11907 ) ;
#3210 = VERTEX_POINT ( 'NONE', #2297 ) ;
#3211 = ORIENTED_EDGE ( 'NONE', *, *, #8678, .F. ) ;
#3212 = ORIENTED_EDGE ( 'NONE', *, *, #6988, .F. ) ;
#3213 = FACE_OUTER_BOUND ( 'NONE', #12606, .T. ) ;
#3214 = VERTEX_POINT ( 'NONE', #1258 ) ;
#3215 = CARTESIAN_POINT ( 'NONE',  ( 1.958204620527036102E-15, -69.99999999999998579, 1.236099792129133461E-16 ) ) ;
#3216 = VECTOR ( 'NONE', #3790, 1000.000000000000000 ) ;
#3217 =( BOUNDED_SURFACE ( )  B_SPLINE_SURFACE ( 3, 3, ( 
 ( #13837, #7274, #10369, #9251 ),
 ( #10500, #1950, #5038, #2802 ),
 ( #13565, #3919, #9321, #12627 ),
 ( #8265, #12558, #7207, #2942 ) ),
 .UNSPECIFIED., .F., .F., .F. ) 
 B_SPLINE_SURFACE_WITH_KNOTS ( ( 4, 4 ),
 ( 4, 4 ),
 ( 0.000000000000000000, 1.000000000000000000 ),
 ( 0.000000000000000000, 1.000000000000000000 ),
 .UNSPECIFIED. ) 
 GEOMETRIC_REPRESENTATION_ITEM ( )  RATIONAL_B_SPLINE_SURFACE ( (
 ( 1.000000000000000000, 0.3333333333333334259, 0.3333333333333334259, 1.000000000000000000),
 ( 1.000000000000000000, 0.3333333333333334259, 0.3333333333333334259, 1.000000000000000000),
 ( 1.000000000000000000, 0.3333333333333334259, 0.3333333333333334259, 1.000000000000000000),
 ( 1.000000000000000000, 0.3333333333333334259, 0.3333333333333334259, 1.000000000000000000) ) ) 
 REPRESENTATION_ITEM ( '' )  SURFACE ( )  );
#3218 = CARTESIAN_POINT ( 'NONE',  ( -35.00000000000000000, 25.00000000000000000, 4.000000000000000000 ) ) ;
#3219 = CARTESIAN_POINT ( 'NONE',  ( 38.99425905299097650, 101.5795188936649112, -2.500000000000004441 ) ) ;
#3220 = CARTESIAN_POINT ( 'NONE',  ( 15.29705854078138572, 66.79670324143890525, 1.757061666260240493E-15 ) ) ;
#3221 = CARTESIAN_POINT ( 'NONE',  ( -7.706471693472447981, -95.44282728834829754, -2.820513248663373496 ) ) ;
#3222 = CARTESIAN_POINT ( 'NONE',  ( 25.00000000000000355, 120.0000000000000284, 0.5000000000000000000 ) ) ;
#3223 = ORIENTED_EDGE ( 'NONE', *, *, #10707, .F. ) ;
#3224 = VECTOR ( 'NONE', #449, 1000.000000000000000 ) ;
#3225 = ORIENTED_EDGE ( 'NONE', *, *, #3340, .F. ) ;
#3226 = CIRCLE ( 'NONE', #13113, 23.64268088454700845 ) ;
#3227 = VECTOR ( 'NONE', #1939, 1000.000000000000000 ) ;
#3228 = CARTESIAN_POINT ( 'NONE',  ( -35.00000000000000000, -4.286263797015736496E-15, -10.49999999999999822 ) ) ;
#3229 = VERTEX_POINT ( 'NONE', #508 ) ;
#3230 = FACE_OUTER_BOUND ( 'NONE', #2196, .T. ) ;
#3231 = DIRECTION ( 'NONE',  ( 0.000000000000000000, 0.000000000000000000, 1.000000000000000000 ) ) ;
#3232 = CARTESIAN_POINT ( 'NONE',  ( -3.339827705271122937, -118.5554015396263878, -4.233164074552941081 ) ) ;
#3233 = CARTESIAN_POINT ( 'NONE',  ( -12.99579180576516002, 7.534841976936127672, -25.99158361153033070 ) ) ;
#3234 = DIRECTION ( 'NONE',  ( 0.9556796851544554494, -0.2944084567112178474, 0.000000000000000000 ) ) ;
#3235 = CIRCLE ( 'NONE', #11082, 42.00000000000001421 ) ;
#3236 = CARTESIAN_POINT ( 'NONE',  ( 0.7701066202684784257, -168.0000000000001421, 1.909695209560601681 ) ) ;
#3237 = CARTESIAN_POINT ( 'NONE',  ( -10.03938689678716045, -69.87878787879108700, -0.2267434780641402192 ) ) ;
#3238 = CARTESIAN_POINT ( 'NONE',  ( 52.27091746333575628, 18.76074118940758595, 2.500000000000006217 ) ) ;
#3239 = TOROIDAL_SURFACE ( 'NONE', #350, 16.99999999999998934, 2.000000000000000000 ) ;
#3240 = DIRECTION ( 'NONE',  ( 1.000000000000000000, 0.000000000000000000, 0.000000000000000000 ) ) ;
#3241 = EDGE_CURVE ( 'NONE', #2953, #8273, #4688, .T. ) ;
#3242 = EDGE_CURVE ( 'NONE', #887, #7475, #6092, .T. ) ;
#3243 = CARTESIAN_POINT ( 'NONE',  ( -24.99999999999998934, -100.0000000000000000, -7.500000000000000000 ) ) ;
#3244 = CARTESIAN_POINT ( 'NONE',  ( 45.97632359910777922, 102.2167537197081657, 7.500000000000000000 ) ) ;
#3245 = ORIENTED_EDGE ( 'NONE', *, *, #12549, .T. ) ;
#3246 = CIRCLE ( 'NONE', #7726, 5.000000000000004441 ) ;
#3247 = ORIENTED_EDGE ( 'NONE', *, *, #3425, .F. ) ;
#3248 = CARTESIAN_POINT ( 'NONE',  ( -1.024862805779478135E-15, 36.63580182200523438, -6.469358145237827718E-17 ) ) ;
#3249 = CIRCLE ( 'NONE', #4366, 9.000000000008999024 ) ;
#3250 = ORIENTED_EDGE ( 'NONE', *, *, #2581, .T. ) ;
#3251 = CARTESIAN_POINT ( 'NONE',  ( -25.00000000000000355, 120.0000000000000142, -0.5000000000000000000 ) ) ;
#3252 = EDGE_LOOP ( 'NONE', ( #9462, #13561, #7871, #3138, #12129, #12946, #13215, #9895 ) ) ;
#3253 = VECTOR ( 'NONE', #12432, 1000.000000000000000 ) ;
#3254 = CARTESIAN_POINT ( 'NONE',  ( -2.517691654963332357E-15, 90.00000000000000000, -1.589271161308885878E-16 ) ) ;
#3255 = CARTESIAN_POINT ( 'NONE',  ( -12.99579180576517601, 26.38439787695498495, 25.99158361153033425 ) ) ;
#3256 = LINE ( 'NONE', #7530, #8783 ) ;
#3257 = CARTESIAN_POINT ( 'NONE',  ( 8.385254915620292238, -22.36966495935058319, 1.068716529980328346E-15 ) ) ;
#3258 = CARTESIAN_POINT ( 'NONE',  ( 15.29705854078138927, 10.24803554138234318, -30.59411708156276788 ) ) ;
#3259 = DIRECTION ( 'NONE',  ( -0.000000000000000000, -0.000000000000000000, -1.000000000000000000 ) ) ;
#3260 = AXIS2_PLACEMENT_3D ( 'NONE', #4239, #5970, #10688 ) ;
#3261 = FACE_OUTER_BOUND ( 'NONE', #1519, .T. ) ;
#3262 = EDGE_CURVE ( 'NONE', #13056, #12412, #33, .T. ) ;
#3263 = FACE_BOUND ( 'NONE', #13106, .T. ) ;
#3264 = EDGE_CURVE ( 'NONE', #2504, #12042, #1531, .T. ) ;
#3265 = AXIS2_PLACEMENT_3D ( 'NONE', #2105, #5604, #5394 ) ;
#3266 = ADVANCED_FACE ( 'NONE', ( #12348 ), #3847, .F. ) ;
#3267 = ORIENTED_EDGE ( 'NONE', *, *, #13761, .T. ) ;
#3268 = ADVANCED_FACE ( 'NONE', ( #3707 ), #9049, .T. ) ;
#3269 = EDGE_CURVE ( 'NONE', #6682, #4795, #12795, .T. ) ;
#3270 = CIRCLE ( 'NONE', #7520, 8.385254915620290461 ) ;
#3271 = ORIENTED_EDGE ( 'NONE', *, *, #9104, .F. ) ;
#3272 = DIRECTION ( 'NONE',  ( -6.158143864569485777E-17, -2.736152283717910599E-16, 1.000000000000000000 ) ) ;
#3273 = DIRECTION ( 'NONE',  ( 0.000000000000000000, 0.000000000000000000, 1.000000000000000000 ) ) ;
#3274 = CYLINDRICAL_SURFACE ( 'NONE', #6073, 2.000000000000001776 ) ;
#3275 = CARTESIAN_POINT ( 'NONE',  ( -25.00000000000000355, 120.0000000000000142, 7.500000000000000000 ) ) ;
#3276 = EDGE_CURVE ( 'NONE', #1407, #13124, #7621, .T. ) ;
#3277 = CARTESIAN_POINT ( 'NONE',  ( 34.99999999999958789, 1.091249486606660213E-13, 2.500000000000000000 ) ) ;
#3278 = VERTEX_POINT ( 'NONE', #361 ) ;
#3279 = PRODUCT ( 'Soft-Touch Grip Cap Sleeve', 'Soft-Touch Grip Cap Sleeve', '', ( #6636 ) ) ;
#3280 = ORIENTED_EDGE ( 'NONE', *, *, #11093, .T. ) ;
#3281 = EDGE_CURVE ( 'NONE', #3625, #3737, #1150, .T. ) ;
#3282 = ORIENTED_EDGE ( 'NONE', *, *, #2082, .F. ) ;
#3283 = CYLINDRICAL_SURFACE ( 'NONE', #3133, 2.000000000000000000 ) ;
#3284 = EDGE_LOOP ( 'NONE', ( #5814, #6647, #8077, #11520 ) ) ;
#3285 = CARTESIAN_POINT ( 'NONE',  ( 12.99579180576516002, 73.50828762700210461, 25.99158361153033425 ) ) ;
#3286 = PLANE ( 'NONE',  #11612 ) ;
#3287 = DIRECTION ( 'NONE',  ( 0.8907235428302473501, -0.4545454545454531425, 0.000000000000000000 ) ) ;
#3288 = LINE ( 'NONE', #9815, #12176 ) ;
#3289 = CARTESIAN_POINT ( 'NONE',  ( -8.193545109616771072, -89.96337882711635814, 3.459978222445851515 ) ) ;
#3290 = CARTESIAN_POINT ( 'NONE',  ( -10.00000000000000711, 92.00000000000000000, 0.5000000000000000000 ) ) ;
#3291 = VERTEX_POINT ( 'NONE', #5894 ) ;
#3292 = ORIENTED_EDGE ( 'NONE', *, *, #3096, .F. ) ;
#3293 = ORIENTED_EDGE ( 'NONE', *, *, #2935, .T. ) ;
#3294 =( BOUNDED_SURFACE ( )  B_SPLINE_SURFACE ( 3, 3, ( 
 ( #3567, #5752, #8986, #9126 ),
 ( #1618, #8074, #13291, #13441 ),
 ( #3930, #12638, #9401, #12493 ),
 ( #11631, #10383, #5051, #10508 ) ),
 .UNSPECIFIED., .F., .F., .F. ) 
 B_SPLINE_SURFACE_WITH_KNOTS ( ( 4, 4 ),
 ( 4, 4 ),
 ( 0.000000000000000000, 1.000000000000000000 ),
 ( 0.000000000000000000, 1.000000000000000000 ),
 .UNSPECIFIED. ) 
 GEOMETRIC_REPRESENTATION_ITEM ( )  RATIONAL_B_SPLINE_SURFACE ( (
 ( 1.000000000000000000, 0.3333333333333334259, 0.3333333333333334259, 1.000000000000000000),
 ( 1.000000000000000000, 0.3333333333333334259, 0.3333333333333334259, 1.000000000000000000),
 ( 1.000000000000000000, 0.3333333333333334259, 0.3333333333333334259, 1.000000000000000000),
 ( 1.000000000000000000, 0.3333333333333334259, 0.3333333333333334259, 1.000000000000000000) ) ) 
 REPRESENTATION_ITEM ( '' )  SURFACE ( )  );
#3295 = CARTESIAN_POINT ( 'NONE',  ( -2.482863863605453414, 89.99999999999998579, 4.353049703108321289 ) ) ;
#3296 = EDGE_LOOP ( 'NONE', ( #1863, #5946, #10075 ) ) ;
#3297 = DIRECTION ( 'NONE',  ( -0.5999999999999989786, -0.8000000000000008216, 0.000000000000000000 ) ) ;
#3298 = CARTESIAN_POINT ( 'NONE',  ( 0.9875500501441598633, -80.00464164738322381, -10.06307372056550342 ) ) ;
#3299 = CARTESIAN_POINT ( 'NONE',  ( -15.29705854078138394, 8.361467971976955127, -30.59411708156277854 ) ) ;
#3300 = FACE_OUTER_BOUND ( 'NONE', #3599, .T. ) ;
#3301 = CARTESIAN_POINT ( 'NONE',  ( -0.04956920568762178403, -160.9696969682810561, 0.4964001826923840621 ) ) ;
#3302 = CARTESIAN_POINT ( 'NONE',  ( -6.967039245478320098, -74.45454545454718698, -7.244513656184790484 ) ) ;
#3303 = CARTESIAN_POINT ( 'NONE',  ( -35.45454545454546036, 140.4866414850956744, -0.5000000000000000000 ) ) ;
#3304 = CARTESIAN_POINT ( 'NONE',  ( 52.26118412238654543, 18.64354822589355365, -2.499999999999993339 ) ) ;
#3305 = AXIS2_PLACEMENT_3D ( 'NONE', #4124, #8272, #2023 ) ;
#3306 = ORIENTED_EDGE ( 'NONE', *, *, #8190, .T. ) ;
#3307 = CIRCLE ( 'NONE', #2190, 22.00000000000000355 ) ;
#3308 = DIRECTION ( 'NONE',  ( -1.000000000000000000, 0.000000000000000000, 0.000000000000000000 ) ) ;
#3309 = DIRECTION ( 'NONE',  ( -0.000000000000000000, -0.000000000000000000, 1.000000000000000000 ) ) ;
#3310 = VERTEX_POINT ( 'NONE', #2594 ) ;
#3311 = DIRECTION ( 'NONE',  ( 0.000000000000000000, 0.000000000000000000, 1.000000000000000000 ) ) ;
#3312 = FACE_OUTER_BOUND ( 'NONE', #6822, .T. ) ;
#3313 = ORIENTED_EDGE ( 'NONE', *, *, #7794, .T. ) ;
#3314 = DIRECTION ( 'NONE',  ( 1.000000000000000000, 1.850371707708595154E-15, 0.000000000000000000 ) ) ;
#3315 = ORIENTED_EDGE ( 'NONE', *, *, #12528, .T. ) ;
#3316 = MANIFOLD_SOLID_BREP ( 'Cavity1', #2210 ) ;
#3317 = DIRECTION ( 'NONE',  ( -1.000000000000000000, 1.224646799147353454E-16, 0.000000000000000000 ) ) ;
#3318 = EDGE_CURVE ( 'NONE', #5305, #1178, #12582, .T. ) ;
#3319 = AXIS2_PLACEMENT_3D ( 'NONE', #13898, #143, #7617 ) ;
#3320 = CARTESIAN_POINT ( 'NONE',  ( 12.99579180576517068, 54.65873172698324112, -25.99158361153033070 ) ) ;
#3321 = CARTESIAN_POINT ( 'NONE',  ( 34.25812584745457201, 108.1980041606221050, -0.5000000000000000000 ) ) ;
#3322 = VECTOR ( 'NONE', #8015, 1000.000000000000000 ) ;
#3323 = DIRECTION ( 'NONE',  ( 1.000000000000000000, 0.000000000000000000, 0.000000000000000000 ) ) ;
#3324 = DIRECTION ( 'NONE',  ( 0.000000000000000000, 0.000000000000000000, 1.000000000000000000 ) ) ;
#3325 =( BOUNDED_SURFACE ( )  B_SPLINE_SURFACE ( 3, 3, ( 
 ( #1522, #423, #4762, #9036 ),
 ( #13350, #3767, #6999, #2649 ),
 ( #11209, #12335, #2725, #11279 ),
 ( #1035, #10564, #10494, #2993 ) ),
 .UNSPECIFIED., .F., .F., .T. ) 
 B_SPLINE_SURFACE_WITH_KNOTS ( ( 4, 4 ),
 ( 4, 4 ),
 ( 0.000000000000000000, 1.000000000000000000 ),
 ( 0.000000000000000000, 1.000000000000000000 ),
 .UNSPECIFIED. ) 
 GEOMETRIC_REPRESENTATION_ITEM ( )  RATIONAL_B_SPLINE_SURFACE ( (
 ( 1.000000000000000000, 0.3333333333333334259, 0.3333333333333334259, 1.000000000000000000),
 ( 1.000000000000000000, 0.3333333333333334259, 0.3333333333333334259, 1.000000000000000000),
 ( 1.000000000000000000, 0.3333333333333334259, 0.3333333333333334259, 1.000000000000000000),
 ( 1.000000000000000000, 0.3333333333333334259, 0.3333333333333334259, 1.000000000000000000) ) ) 
 REPRESENTATION_ITEM ( '' )  SURFACE ( )  );
#3326 = CARTESIAN_POINT ( 'NONE',  ( 25.00000000000000355, 120.0000000000000142, -2.500000000000000000 ) ) ;
#3327 = CARTESIAN_POINT ( 'NONE',  ( 34.99999999999958789, 1.104930248025249758E-13, -2.499999999999999112 ) ) ;
#3328 = CARTESIAN_POINT ( 'NONE',  ( -12.99579180576517068, 16.95961992694555676, 25.99158361153032359 ) ) ;
#3329 = AXIS2_PLACEMENT_3D ( 'NONE', #804, #5074, #9283 ) ;
#3330 = ORIENTED_EDGE ( 'NONE', *, *, #11633, .F. ) ;
#3331 = ORIENTED_EDGE ( 'NONE', *, *, #13794, .T. ) ;
#3332 = ADVANCED_FACE ( 'NONE', ( #8463 ), #1813, .T. ) ;
#3333 =( NAMED_UNIT ( * ) SI_UNIT ( $, .STERADIAN. ) SOLID_ANGLE_UNIT ( ) );
#3334 = EDGE_CURVE ( 'NONE', #2559, #3663, #6972, .T. ) ;
#3335 = VERTEX_POINT ( 'NONE', #13637 ) ;
#3336 = DIRECTION ( 'NONE',  ( -0.000000000000000000, -0.000000000000000000, -1.000000000000000000 ) ) ;
#3337 = AXIS2_PLACEMENT_3D ( 'NONE', #11385, #12246, #9227 ) ;
#3338 = CARTESIAN_POINT ( 'NONE',  ( 25.00000000000002132, -99.17107372196666404, 0.8524342262973642059 ) ) ;
#3339 = ADVANCED_FACE ( 'NONE', ( #6301 ), #6623, .T. ) ;
#3340 = EDGE_CURVE ( 'NONE', #3968, #5518, #6513, .T. ) ;
#3341 = CARTESIAN_POINT ( 'NONE',  ( 34.99999999999958789, 1.104930248025249758E-13, -2.499999999999999112 ) ) ;
#3342 = TOROIDAL_SURFACE ( 'NONE', #1781, 22.99999999999999289, 2.000000000000000000 ) ;
#3343 = CYLINDRICAL_SURFACE ( 'NONE', #3319, 8.385254915620292238 ) ;
#3344 = ORIENTED_EDGE ( 'NONE', *, *, #8677, .T. ) ;
#3345 = TOROIDAL_SURFACE ( 'NONE', #6937, 3.999999999999998224, 2.000000000000000000 ) ;
#3346 = AXIS2_PLACEMENT_3D ( 'NONE', #13034, #11044, #8801 ) ;
#3347 = VERTEX_POINT ( 'NONE', #13707 ) ;
#3348 = EDGE_LOOP ( 'NONE', ( #6645, #12608, #279, #11906 ) ) ;
#3349 = ORIENTED_EDGE ( 'NONE', *, *, #4817, .T. ) ;
#3350 = CARTESIAN_POINT ( 'NONE',  ( -8.385254915620292238, 71.87811454074363837, 16.77050983124057382 ) ) ;
#3351 = CARTESIAN_POINT ( 'NONE',  ( 25.00000000000000355, 120.0000000000000284, 2.500000000000000000 ) ) ;
#3352 = CARTESIAN_POINT ( 'NONE',  ( 35.00000000000000000, 4.286263797015736496E-15, -7.500000000000000000 ) ) ;
#3353 = ADVANCED_FACE ( 'NONE', ( #5238 ), #3217, .T. ) ;
#3354 = CARTESIAN_POINT ( 'NONE',  ( -34.40223077810360763, 107.7696006147693026, -1.740676078835883045 ) ) ;
#3355 = CYLINDRICAL_SURFACE ( 'NONE', #1412, 8.385254915620295790 ) ;
#3356 = AXIS2_PLACEMENT_3D ( 'NONE', #7845, #4691, #3483 ) ;
#3357 = DIRECTION ( 'NONE',  ( -0.000000000000000000, -0.000000000000000000, -1.000000000000000000 ) ) ;
#3358 = CARTESIAN_POINT ( 'NONE',  ( 0.000000000000000000, 71.01020514433645303, 0.5000000000000000000 ) ) ;
#3359 = ORIENTED_EDGE ( 'NONE', *, *, #5951, .F. ) ;
#3360 = AXIS2_PLACEMENT_3D ( 'NONE', #1521, #11206, #7060 ) ;
#3361 = ORIENTED_EDGE ( 'NONE', *, *, #9436, .T. ) ;
#3362 = ORIENTED_EDGE ( 'NONE', *, *, #6959, .F. ) ;
#3363 = CARTESIAN_POINT ( 'NONE',  ( 9.857979974958242408, 4.257796268226279324, 8.673617379884035472E-16 ) ) ;
#3364 = MECHANICAL_DESIGN_GEOMETRIC_PRESENTATION_REPRESENTATION (  '', ( #1595 ), #8521 ) ;
#3365 = CARTESIAN_POINT ( 'NONE',  ( 48.99302833075611119, 12.47878836808090064, -2.499999999999994671 ) ) ;
#3366 = ORIENTED_EDGE ( 'NONE', *, *, #6659, .F. ) ;
#3367 = LINE ( 'NONE', #11993, #313 ) ;
#3368 = CARTESIAN_POINT ( 'NONE',  ( -15.29705854078139460, 36.63580182200524149, 30.59411708156277498 ) ) ;
#3369 = CARTESIAN_POINT ( 'NONE',  ( 15.01254563088791372, -15.83514028494776760, -5.204170427930421283E-15 ) ) ;
#3370 = CARTESIAN_POINT ( 'NONE',  ( 34.99999999999958789, 1.104930248025249758E-13, -2.499999999999999112 ) ) ;
#3371 = CARTESIAN_POINT ( 'NONE',  ( -0.4692480219583425871, -80.00113634546181629, -9.989149782162604296 ) ) ;
#3372 = CARTESIAN_POINT ( 'NONE',  ( -1.830305755785371247, -166.5454545179101444, -12.49768923203297000 ) ) ;
#3373 = EDGE_CURVE ( 'NONE', #3769, #12961, #927, .T. ) ;
#3374 = CARTESIAN_POINT ( 'NONE',  ( -0.1760972876107445573, -80.66666666666708352, -10.02690338805403059 ) ) ;
#3375 = CARTESIAN_POINT ( 'NONE',  ( 34.99999999999958789, 1.104930248025249758E-13, -2.499999999999999112 ) ) ;
#3376 = CARTESIAN_POINT ( 'NONE',  ( 30.92745768374916082, -20.74715399464528787, -2.500000000000005329 ) ) ;
#3377 = ORIENTED_EDGE ( 'NONE', *, *, #11978, .T. ) ;
#3378 = AXIS2_PLACEMENT_3D ( 'NONE', #12095, #9997, #405 ) ;
#3379 = DIRECTION ( 'NONE',  ( -6.158143864569485777E-17, -2.736152283717910599E-16, 1.000000000000000000 ) ) ;
#3380 = DIRECTION ( 'NONE',  ( 6.158143864569485777E-17, 2.736152283717910599E-16, -1.000000000000000000 ) ) ;
#3381 = DIRECTION ( 'NONE',  ( -1.000000000000000000, 0.000000000000000000, 0.000000000000000000 ) ) ;
#3382 = DIRECTION ( 'NONE',  ( -2.797435172181481150E-17, 1.000000000000000000, -1.765856845898762549E-18 ) ) ;
#3383 = ORIENTED_EDGE ( 'NONE', *, *, #11733, .T. ) ;
#3384 = CARTESIAN_POINT ( 'NONE',  ( 35.45454545454547457, 140.4866414850956460, -0.5000000000000000000 ) ) ;
#3385 = LINE ( 'NONE', #2484, #4352 ) ;
#3386 = CARTESIAN_POINT ( 'NONE',  ( 34.99999999999958789, 1.104930248025249758E-13, -2.499999999999999112 ) ) ;
#3387 = CARTESIAN_POINT ( 'NONE',  ( 34.33120614476064958, 107.9646345552176001, -1.436946644489084157 ) ) ;
#3388 = B_SPLINE_SURFACE_WITH_KNOTS ( 'NONE', 3, 3, ( 
 ( #12939, #3439, #7448, #6603, #9829, #10937, #9764, #13874, #173, #1155, #4219, #11728, #4498, #10868 ),
 ( #3173, #3374, #8776, #13087, #2118, #9563, #6406, #10673, #7581, #5281, #1083, #3237, #7516, #11864 ),
 ( #2389, #8574, #5542, #5345, #9631, #38, #4292, #3302, #2259, #12873, #1215, #11797, #6542, #2186 ),
 ( #6471, #10738, #5411, #9694, #102, #4418, #4354, #13007, #8638, #10800, #5479, #8702, #13691, #559 ) ),
 .UNSPECIFIED., .F., .F., .F.,
 ( 4, 4 ),
 ( 4, 1, 1, 1, 1, 1, 1, 1, 1, 1, 1, 4 ),
 ( -0.003299999999999999982, 0.0002999999999999999195 ),
 ( 0.07900000000000000078, 0.08000000000000000167, 0.08063636363636363102, 0.08172727272727271786, 0.08336363636363636198, 0.08445454545454544881, 0.08554545454545453564, 0.08663636363636362248, 0.08827272727272726660, 0.08936363636363635343, 0.08999999999999998279, 0.09099999999999998368 ),
 .UNSPECIFIED. ) ;
#3389 = AXIS2_PLACEMENT_3D ( 'NONE', #10518, #9204, #8149 ) ;
#3390 = CARTESIAN_POINT ( 'NONE',  ( -25.00000000000000355, 120.0000000000000142, -2.499999999999998668 ) ) ;
#3391 = DIRECTION ( 'NONE',  ( -0.7999999999999996003, -0.6000000000000007550, 0.000000000000000000 ) ) ;
#3392 = CARTESIAN_POINT ( 'NONE',  ( -31.00000000000000711, -4.286263797015736496E-15, 10.49999999999999822 ) ) ;
#3393 = DIRECTION ( 'NONE',  ( 0.9960067511297463483, -0.08927794634716620936, 4.626175998653454121E-17 ) ) ;
#3394 = FACE_OUTER_BOUND ( 'NONE', #445, .T. ) ;
#3395 = ADVANCED_FACE ( 'NONE', ( #10438 ), #839, .T. ) ;
#3396 = DIRECTION ( 'NONE',  ( 1.000000000000000000, 0.000000000000000000, 0.000000000000000000 ) ) ;
#3397 = ORIENTED_EDGE ( 'NONE', *, *, #543, .F. ) ;
#3398 = CARTESIAN_POINT ( 'NONE',  ( -35.00000000000000000, -4.286263797015736496E-15, 4.000000000000000000 ) ) ;
#3399 = ORIENTED_EDGE ( 'NONE', *, *, #12828, .F. ) ;
#3400 = DIRECTION ( 'NONE',  ( -1.000000000000000000, 0.000000000000000000, 0.000000000000000000 ) ) ;
#3401 = EDGE_LOOP ( 'NONE', ( #8208, #7217, #74, #1560 ) ) ;
#3402 = CARTESIAN_POINT ( 'NONE',  ( -15.29705854078139105, 27.21102387199583816, -4.805077278827845308E-17 ) ) ;
#3403 = DIRECTION ( 'NONE',  ( -0.000000000000000000, -1.000000000000000000, -0.000000000000000000 ) ) ;
#3404 = AXIS2_PLACEMENT_3D ( 'NONE', #5505, #9789, #262 ) ;
#3405 = DIRECTION ( 'NONE',  ( 1.000000000000000000, 3.495146559005123961E-15, 0.000000000000000000 ) ) ;
#3406 = CARTESIAN_POINT ( 'NONE',  ( 10.69346802281033959, 11.89973432371241202, 21.38693604562068984 ) ) ;
#3407 = EDGE_LOOP ( 'NONE', ( #8138, #12920, #11329, #10765 ) ) ;
#3408 = EDGE_CURVE ( 'NONE', #8113, #12059, #3837, .T. ) ;
#3409 = ORIENTED_EDGE ( 'NONE', *, *, #10824, .F. ) ;
#3410 = ADVANCED_FACE ( 'NONE', ( #1044 ), #6365, .T. ) ;
#3411 = AXIS2_PLACEMENT_3D ( 'NONE', #10087, #6785, #11137 ) ;
#3412 = ADVANCED_FACE ( 'NONE', ( #10634 ), #13513, .F. ) ;
#3413 = B_SPLINE_CURVE_WITH_KNOTS ( 'NONE', 3,
 ( #4985, #12573, #3933, #13847, #10318, #11436, #4129, #11634, #12769, #4191, #9261, #10387, #12706, #2031, #6114, #8475 ),
 .UNSPECIFIED., .F., .F.,
 ( 4, 2, 2, 2, 2, 2, 2, 4 ),
 ( 0.000000000000000000, 0.0005014865247272646664, 0.001002973049454529333, 0.001504459574181793999, 0.002005946098909058666, 0.002507432623636323549, 0.003008919148363587998, 0.004011892197818117331 ),
 .UNSPECIFIED. ) ;
#3414 = CARTESIAN_POINT ( 'NONE',  ( 1.031578115675553693E-15, -36.87585420866476227, 6.511747960273540061E-17 ) ) ;
#3415 = ORIENTED_EDGE ( 'NONE', *, *, #2985, .F. ) ;
#3416 = CARTESIAN_POINT ( 'NONE',  ( 55.16425081158429577, -10.83695794929873912, -2.500000000000000888 ) ) ;
#3417 = AXIS2_PLACEMENT_3D ( 'NONE', #3936, #13851, #1965 ) ;
#3418 = DIRECTION ( 'NONE',  ( -2.797435172181481150E-17, 1.000000000000000000, -1.765856845898762549E-18 ) ) ;
#3419 = CIRCLE ( 'NONE', #4543, 2.500000000000000444 ) ;
#3420 = CARTESIAN_POINT ( 'NONE',  ( -0.2039587671352304787, -79.18543995220413478, -10.12004280472452322 ) ) ;
#3421 = DIRECTION ( 'NONE',  ( -6.158143864569485777E-17, -2.736152283717910599E-16, 1.000000000000000000 ) ) ;
#3422 = CARTESIAN_POINT ( 'NONE',  ( 39.99999999999999289, 120.0000000000000284, 0.5000000000000000000 ) ) ;
#3423 = CARTESIAN_POINT ( 'NONE',  ( -2.627534660932791866, -83.45264110882523312, 9.274001503740121777 ) ) ;
#3424 = CARTESIAN_POINT ( 'NONE',  ( 52.82363224725100537, -5.817485239812894449, -2.500000000000000000 ) ) ;
#3425 = EDGE_CURVE ( 'NONE', #2956, #8890, #4272, .T. ) ;
#3426 = ORIENTED_EDGE ( 'NONE', *, *, #1994, .T. ) ;
#3427 = ADVANCED_FACE ( 'NONE', ( #3201 ), #7479, .T. ) ;
#3428 = ORIENTED_EDGE ( 'NONE', *, *, #10419, .F. ) ;
#3429 = EDGE_CURVE ( 'NONE', #8021, #11572, #6753, .T. ) ;
#3430 = CIRCLE ( 'NONE', #10392, 2.000000000000003109 ) ;
#3431 = EDGE_CURVE ( 'NONE', #6129, #5860, #7415, .T. ) ;
#3432 = DIRECTION ( 'NONE',  ( -0.000000000000000000, -0.000000000000000000, -1.000000000000000000 ) ) ;
#3433 = VERTEX_POINT ( 'NONE', #11760 ) ;
#3434 = CARTESIAN_POINT ( 'NONE',  ( 12.99579180576516002, -1.889935973073298081, 25.99158361153033070 ) ) ;
#3435 = CARTESIAN_POINT ( 'NONE',  ( -42.16244658108819010, 105.4500712252157797, -2.499999999999998668 ) ) ;
#3436 = DIRECTION ( 'NONE',  ( -6.158143864569485777E-17, -2.736152283717910599E-16, 1.000000000000000000 ) ) ;
#3437 = DIRECTION ( 'NONE',  ( -6.158143864569485777E-17, -2.736152283717910599E-16, 1.000000000000000000 ) ) ;
#3438 = CARTESIAN_POINT ( 'NONE',  ( 0.9182679296299990357, -167.9999999999998863, 0.7188769083877146748 ) ) ;
#3439 = CARTESIAN_POINT ( 'NONE',  ( -1.376272962219557749, -80.66666666666647245, -10.07778225401753147 ) ) ;
#3440 = CARTESIAN_POINT ( 'NONE',  ( -25.00000000000000355, 120.0000000000000142, 2.500000000000000000 ) ) ;
#3441 = AXIS2_PLACEMENT_3D ( 'NONE', #12258, #6914, #3834 ) ;
#3442 = EDGE_CURVE ( 'NONE', #9172, #11147, #1504, .T. ) ;
#3443 = ORIENTED_EDGE ( 'NONE', *, *, #969, .T. ) ;
#3444 = DIRECTION ( 'NONE',  ( 0.000000000000000000, 1.000000000000000000, 0.000000000000000000 ) ) ;
#3445 = DIRECTION ( 'NONE',  ( -5.551115123125776539E-17, 1.000000000000000000, 3.204747427460360459E-31 ) ) ;
#3446 = ORIENTED_EDGE ( 'NONE', *, *, #7911, .F. ) ;
#3447 = FACE_OUTER_BOUND ( 'NONE', #1254, .T. ) ;
#3448 = ADVANCED_FACE ( 'NONE', ( #10696 ), #8062, .T. ) ;
#3449 = DIRECTION ( 'NONE',  ( -2.797435172181481150E-17, 1.000000000000000000, -1.765856845898762549E-18 ) ) ;
#3450 = DIRECTION ( 'NONE',  ( -0.3926913852462016186, -0.9196703082917373484, -2.891205793291787644E-16 ) ) ;
#3451 = ORIENTED_EDGE ( 'NONE', *, *, #6098, .T. ) ;
#3452 = AXIS2_PLACEMENT_3D ( 'NONE', #4306, #6349, #4103 ) ;
#3453 = DIRECTION ( 'NONE',  ( -1.000000000000000000, 0.000000000000000000, 0.000000000000000000 ) ) ;
#3454 = EDGE_LOOP ( 'NONE', ( #9211, #12621, #11759, #7218 ) ) ;
#3455 = CARTESIAN_POINT ( 'NONE',  ( 6.991987007918878033E-16, -24.99427717735608212, 4.413631546192547049E-17 ) ) ;
#3456 = CARTESIAN_POINT ( 'NONE',  ( 48.00000000000000000, 120.0000000000000284, 0.5000000000000000000 ) ) ;
#3457 = CARTESIAN_POINT ( 'NONE',  ( 10.69381717166375445, 44.40900277213413716, 1.251590067034001600E-15 ) ) ;
#3458 = VECTOR ( 'NONE', #5220, 1000.000000000000000 ) ;
#3459 = DIRECTION ( 'NONE',  ( 1.000000000000000000, 0.000000000000000000, 0.000000000000000000 ) ) ;
#3460 = CARTESIAN_POINT ( 'NONE',  ( -40.05714107113526978, 100.9137399031062756, -2.016203456813715267 ) ) ;
#3461 = CARTESIAN_POINT ( 'NONE',  ( 39.42607625790186887, 101.2633694847512658, 2.396914520158670570 ) ) ;
#3462 = FACE_OUTER_BOUND ( 'NONE', #7527, .T. ) ;
#3463 = PLANE ( 'NONE',  #10938 ) ;
#3464 = VECTOR ( 'NONE', #249, 1000.000000000000000 ) ;
#3465 = AXIS2_PLACEMENT_3D ( 'NONE', #11722, #3231, #7510 ) ;
#3466 = CIRCLE ( 'NONE', #5723, 42.00000000000001421 ) ;
#3467 = ORIENTED_EDGE ( 'NONE', *, *, #11589, .F. ) ;
#3468 = DIRECTION ( 'NONE',  ( -2.797435172181481150E-17, 1.000000000000000000, -1.765856845898762549E-18 ) ) ;
#3469 = VERTEX_POINT ( 'NONE', #9922 ) ;
#3470 = AXIS2_PLACEMENT_3D ( 'NONE', #12013, #7589, #9705 ) ;
#3471 = DIRECTION ( 'NONE',  ( -1.000000000000000000, 0.000000000000000000, 0.000000000000000000 ) ) ;
#3472 = CARTESIAN_POINT ( 'NONE',  ( 22.00000000000002132, -97.00000000000000000, 7.500000000000000000 ) ) ;
#3473 = AXIS2_PLACEMENT_3D ( 'NONE', #11960, #11202, #3764 ) ;
#3474 = CARTESIAN_POINT ( 'NONE',  ( 40.81228451836345528, 100.6358150620708329, -0.5000000000000000000 ) ) ;
#3475 = DIRECTION ( 'NONE',  ( 0.9960067511297464593, -0.08927794634716622324, 3.401418580343279473E-17 ) ) ;
#3476 = ORIENTED_EDGE ( 'NONE', *, *, #7609, .T. ) ;
#3477 = TOROIDAL_SURFACE ( 'NONE', #6410, 17.49999999999999289, 5.000000000000000000 ) ;
#3478 = ORIENTED_EDGE ( 'NONE', *, *, #4916, .T. ) ;
#3479 = ORIENTED_EDGE ( 'NONE', *, *, #4535, .T. ) ;
#3480 = DIRECTION ( 'NONE',  ( 0.8907235428302473501, 0.4545454545454531425, -6.308085367188369928E-15 ) ) ;
#3481 = AXIS2_PLACEMENT_3D ( 'NONE', #9716, #7600, #6625 ) ;
#3482 = DIRECTION ( 'NONE',  ( 0.000000000000000000, 0.000000000000000000, -1.000000000000000000 ) ) ;
#3483 = DIRECTION ( 'NONE',  ( 0.000000000000000000, 0.000000000000000000, 1.000000000000000000 ) ) ;
#3484 = CARTESIAN_POINT ( 'NONE',  ( -34.27523635402735636, 108.1397967565349916, -0.9870360185550085541 ) ) ;
#3485 = CARTESIAN_POINT ( 'NONE',  ( 41.86252833142972918, 24.55922850786694056, -2.499999999999992450 ) ) ;
#3486 = CARTESIAN_POINT ( 'NONE',  ( -12.99579180576517423, -30.16426982310158067, -3.167125725528906618E-15 ) ) ;
#3487 = LINE ( 'NONE', #293, #10647 ) ;
#3488 = VERTEX_POINT ( 'NONE', #327 ) ;
#3489 = VERTEX_POINT ( 'NONE', #4583 ) ;
#3490 = VERTEX_POINT ( 'NONE', #7804 ) ;
#3491 = DIRECTION ( 'NONE',  ( 0.9928035427100112553, 0.1197544386753605361, 9.637352644305958814E-17 ) ) ;
#3492 = DIRECTION ( 'NONE',  ( -2.797435172181481150E-17, 1.000000000000000000, -1.765856845898762549E-18 ) ) ;
#3493 = ORIENTED_EDGE ( 'NONE', *, *, #2852, .T. ) ;
#3494 = DIRECTION ( 'NONE',  ( -6.158143864569485777E-17, -2.736152283717910599E-16, 1.000000000000000000 ) ) ;
#3495 = DIRECTION ( 'NONE',  ( 0.000000000000000000, 0.000000000000000000, 1.000000000000000000 ) ) ;
#3496 = CARTESIAN_POINT ( 'NONE',  ( 10.69346802281034314, 59.02362407375952102, 1.239914983259925247E-15 ) ) ;
#3497 = EDGE_CURVE ( 'NONE', #12645, #1929, #5913, .T. ) ;
#3498 = DIRECTION ( 'NONE',  ( -0.000000000000000000, -0.000000000000000000, -1.000000000000000000 ) ) ;
#3499 = CARTESIAN_POINT ( 'NONE',  ( 5.390560935658633923, -117.0909090909101451, 3.329211565281263940 ) ) ;
#3500 = CARTESIAN_POINT ( 'NONE',  ( -25.00000000000000355, 120.0000000000000142, 7.500000000000000000 ) ) ;
#3501 = CARTESIAN_POINT ( 'NONE',  ( -8.385254915620294014, -15.56949922734665570, -2.023984266965477934E-15 ) ) ;
#3502 = DIRECTION ( 'NONE',  ( -1.000000000000000000, 0.000000000000000000, 0.000000000000000000 ) ) ;
#3503 = EDGE_CURVE ( 'NONE', #7000, #5403, #1159, .T. ) ;
#3504 = CARTESIAN_POINT ( 'NONE',  ( -15.18222645069203303, 20.00000000000000000, -4.000000000000000000 ) ) ;
#3505 = DIRECTION ( 'NONE',  ( 1.000000000000000000, 1.224646799147353454E-16, 0.000000000000000000 ) ) ;
#3506 = EDGE_CURVE ( 'NONE', #2436, #9570, #505, .T. ) ;
#3507 = CARTESIAN_POINT ( 'NONE',  ( 0.000000000000000000, 71.01020514433645303, 2.500000000000000000 ) ) ;
#3508 = EDGE_CURVE ( 'NONE', #11915, #9823, #3606, .T. ) ;
#3509 = B_SPLINE_CURVE_WITH_KNOTS ( 'NONE', 3,
 ( #9457, #7202, #834, #897 ),
 .UNSPECIFIED., .F., .F.,
 ( 4, 4 ),
 ( 0.000000000000000000, 1.000000000000000000 ),
 .UNSPECIFIED. ) ;
#3510 = ORIENTED_EDGE ( 'NONE', *, *, #3869, .F. ) ;
#3511 = ORIENTED_EDGE ( 'NONE', *, *, #8678, .T. ) ;
#3512 = CARTESIAN_POINT ( 'NONE',  ( 30.92745768374916082, -20.74715399464528787, 2.499999999999993783 ) ) ;
#3513 = DIRECTION ( 'NONE',  ( 0.000000000000000000, 0.000000000000000000, 1.000000000000000000 ) ) ;
#3514 = CARTESIAN_POINT ( 'NONE',  ( 34.99999999999958789, 1.104930248025249758E-13, -2.499999999999999112 ) ) ;
#3515 = CARTESIAN_POINT ( 'NONE',  ( -24.99999999999999289, -99.72710464630432625, -4.238242954203594870 ) ) ;
#3516 = CARTESIAN_POINT ( 'NONE',  ( -30.72062512117240018, 25.13835616439069653, -4.000000000000000000 ) ) ;
#3517 = EDGE_LOOP ( 'NONE', ( #13594, #12178, #4345, #11699 ) ) ;
#3518 = VERTEX_POINT ( 'NONE', #13540 ) ;
#3519 = CARTESIAN_POINT ( 'NONE',  ( 41.49999999999999289, 98.00000000000001421, 2.499999999999999556 ) ) ;
#3520 = ORIENTED_EDGE ( 'NONE', *, *, #13836, .F. ) ;
#3521 = DIRECTION ( 'NONE',  ( 1.000000000000000000, 3.469446951953614978E-15, 0.000000000000000000 ) ) ;
#3522 = CARTESIAN_POINT ( 'NONE',  ( 4.390129302555905610, 91.34360472797649777, -2.393760519723236779 ) ) ;
#3523 = CARTESIAN_POINT ( 'NONE',  ( 10.69381717166375800, 44.40900277213413716, -21.38763434332750890 ) ) ;
#3524 = DIRECTION ( 'NONE',  ( -6.158143864569485777E-17, -2.736152283717910599E-16, 1.000000000000000000 ) ) ;
#3525 = DIRECTION ( 'NONE',  ( 0.6000000000000001998, 0.7999999999999999334, -0.000000000000000000 ) ) ;
#3526 = CARTESIAN_POINT ( 'NONE',  ( -39.31542348013558552, 101.3376241895501977, -2.435478634890661631 ) ) ;
#3527 = CARTESIAN_POINT ( 'NONE',  ( -13.79311422413708499, -20.00000000000000355, 7.500000000000000000 ) ) ;
#3528 = CARTESIAN_POINT ( 'NONE',  ( 8.385254915620295790, -31.79444290936001138, 2.053795118489800793E-15 ) ) ;
#3529 = CIRCLE ( 'NONE', #13449, 18.74900000001875355 ) ;
#3530 = ADVANCED_FACE ( 'NONE', ( #9150 ), #2905, .T. ) ;
#3531 = DIRECTION ( 'NONE',  ( -0.9960067511297463483, 0.08927794634716619548, 0.000000000000000000 ) ) ;
#3532 = FACE_OUTER_BOUND ( 'NONE', #1448, .T. ) ;
#3533 = ORIENTED_EDGE ( 'NONE', *, *, #5232, .F. ) ;
#3534 = CIRCLE ( 'NONE', #4672, 27.49999999999998579 ) ;
#3535 = VERTEX_POINT ( 'NONE', #8105 ) ;
#3536 = DIRECTION ( 'NONE',  ( -0.000000000000000000, -0.000000000000000000, -1.000000000000000000 ) ) ;
#3537 = CONTEXT_DEPENDENT_SHAPE_REPRESENTATION ( #13767, #2276 ) ;
#3538 = EDGE_LOOP ( 'NONE', ( #9002, #13427, #6946 ) ) ;
#3539 = CARTESIAN_POINT ( 'NONE',  ( -25.00000000000000355, 120.0000000000000142, 7.500000000000000000 ) ) ;
#3540 = DIRECTION ( 'NONE',  ( 0.9960067511297463483, -0.08927794634716620936, 4.626175998653454121E-17 ) ) ;
#3541 = DIRECTION ( 'NONE',  ( 0.000000000000000000, 0.000000000000000000, 1.000000000000000000 ) ) ;
#3542 = EDGE_CURVE ( 'NONE', #2048, #4278, #3821, .T. ) ;
#3543 = CARTESIAN_POINT ( 'NONE',  ( 35.66405164569891184, -18.73723662690267133, -2.500000000000004441 ) ) ;
#3544 = AXIS2_PLACEMENT_3D ( 'NONE', #13497, #7987, #7755 ) ;
#3545 = CARTESIAN_POINT ( 'NONE',  ( 3.164093758375789989, -79.18419793333841028, 9.628149030606312664 ) ) ;
#3546 = ADVANCED_BREP_SHAPE_REPRESENTATION ( '', ( #7695, #8193 ), #5278 ) ;
#3547 = EDGE_LOOP ( 'NONE', ( #13830, #688, #7566, #1189 ) ) ;
#3548 = EDGE_CURVE ( 'NONE', #7192, #3769, #11237, .T. ) ;
#3549 = PRESENTATION_STYLE_ASSIGNMENT (( #12121 ) ) ;
#3550 = VERTEX_POINT ( 'NONE', #8233 ) ;
#3551 = DIRECTION ( 'NONE',  ( -1.000000000000000000, 0.000000000000000000, 0.000000000000000000 ) ) ;
#3552 = CIRCLE ( 'NONE', #5352, 27.49999999999999289 ) ;
#3553 = ORIENTED_EDGE ( 'NONE', *, *, #2516, .T. ) ;
#3554 = ORIENTED_EDGE ( 'NONE', *, *, #6621, .T. ) ;
#3555 = DIRECTION ( 'NONE',  ( 0.000000000000000000, 0.000000000000000000, 1.000000000000000000 ) ) ;
#3556 = CARTESIAN_POINT ( 'NONE',  ( 42.16244658108817589, 105.4500712252157655, 7.500000000000000000 ) ) ;
#3557 = DIRECTION ( 'NONE',  ( -6.158143864569485777E-17, -2.736152283717910599E-16, 1.000000000000000000 ) ) ;
#3558 = CARTESIAN_POINT ( 'NONE',  ( -34.50080218526780129, 107.5336849384756164, 2.002074976903569059 ) ) ;
#3559 = DIRECTION ( 'NONE',  ( -0.000000000000000000, -0.000000000000000000, -1.000000000000000000 ) ) ;
#3560 = FACE_OUTER_BOUND ( 'NONE', #7152, .T. ) ;
#3561 = AXIS2_PLACEMENT_3D ( 'NONE', #12803, #6404, #7245 ) ;
#3562 = ORIENTED_EDGE ( 'NONE', *, *, #13243, .T. ) ;
#3563 = ORIENTED_EDGE ( 'NONE', *, *, #7336, .F. ) ;
#3564 = VECTOR ( 'NONE', #6964, 1000.000000000000000 ) ;
#3565 = EDGE_CURVE ( 'NONE', #1961, #4883, #13474, .T. ) ;
#3566 = AXIS2_PLACEMENT_3D ( 'NONE', #1406, #6661, #10927 ) ;
#3567 = CARTESIAN_POINT ( 'NONE',  ( -8.385254915620297567, -6.144721277337256815, -1.005196162977448937E-15 ) ) ;
#3568 = CYLINDRICAL_SURFACE ( 'NONE', #13568, 79.99999999999997158 ) ;
#3569 = CARTESIAN_POINT ( 'NONE',  ( -1.485233070515140197, -80.99999999999981526, 9.907277990170733517 ) ) ;
#3570 = ORIENTED_EDGE ( 'NONE', *, *, #9107, .F. ) ;
#3571 = CARTESIAN_POINT ( 'NONE',  ( -42.16244658108819010, 105.4500712252157797, 2.499999999999999556 ) ) ;
#3572 = CARTESIAN_POINT ( 'NONE',  ( -15.29705854078139105, 57.37192529142945574, -3.849675066834626958E-15 ) ) ;
#3573 = DIRECTION ( 'NONE',  ( -0.6001121574638169642, 0.7999158696163758409, 1.927470528861191270E-16 ) ) ;
#3574 = AXIS2_PLACEMENT_3D ( 'NONE', #6034, #11423, #4121 ) ;
#3575 = DIRECTION ( 'NONE',  ( -6.158143864569485777E-17, -2.736152283717910599E-16, 1.000000000000000000 ) ) ;
#3576 = CARTESIAN_POINT ( 'NONE',  ( 10.69346802281034847, -16.37459952631584059, 1.341678554766028988E-15 ) ) ;
#3577 = CARTESIAN_POINT ( 'NONE',  ( 2.889799813501469306, -137.4545454544992822, 1.105612428329187047 ) ) ;
#3578 = CIRCLE ( 'NONE', #12786, 16.99999999999998934 ) ;
#3579 = FACE_OUTER_BOUND ( 'NONE', #415, .T. ) ;
#3580 = TOROIDAL_SURFACE ( 'NONE', #4252, 22.49999999999998934, 5.000000000000000000 ) ;
#3581 = DIRECTION ( 'NONE',  ( -0.000000000000000000, -0.000000000000000000, -1.000000000000000000 ) ) ;
#3582 = CARTESIAN_POINT ( 'NONE',  ( -32.50000000000000000, 110.0000000000000142, 7.500000000000000000 ) ) ;
#3583 = EDGE_LOOP ( 'NONE', ( #5772, #5608, #6832, #5918 ) ) ;
#3584 = ORIENTED_EDGE ( 'NONE', *, *, #725, .T. ) ;
#3585 = EDGE_LOOP ( 'NONE', ( #2735, #3932, #12125, #5749 ) ) ;
#3586 = LINE ( 'NONE', #7875, #3564 ) ;
#3587 = ORIENTED_EDGE ( 'NONE', *, *, #9954, .F. ) ;
#3588 = ADVANCED_FACE ( 'NONE', ( #12314 ), #2492, .T. ) ;
#3589 = DIRECTION ( 'NONE',  ( 1.000000000000000000, 0.000000000000000000, 0.000000000000000000 ) ) ;
#3590 = FACE_OUTER_BOUND ( 'NONE', #7836, .T. ) ;
#3591 = TOROIDAL_SURFACE ( 'NONE', #245, 72.49999999999998579, 5.000000000000000000 ) ;
#3592 = CIRCLE ( 'NONE', #1368, 9.000000000009000800 ) ;
#3593 = DIRECTION ( 'NONE',  ( 1.000000000000000000, 3.469446951953615372E-15, 0.000000000000000000 ) ) ;
#3594 = CARTESIAN_POINT ( 'NONE',  ( 38.79999999999999716, 101.5999999999999943, -0.5000000000000000000 ) ) ;
#3595 = ADVANCED_FACE ( 'NONE', ( #6139 ), #12388, .T. ) ;
#3596 = ORIENTED_EDGE ( 'NONE', *, *, #13870, .T. ) ;
#3597 = ORIENTED_EDGE ( 'NONE', *, *, #5751, .T. ) ;
#3598 = CARTESIAN_POINT ( 'NONE',  ( -8.385254915620292238, 71.87811454074363837, -1.269264606320675724E-16 ) ) ;
#3599 = EDGE_LOOP ( 'NONE', ( #9568, #7347, #2129, #8200 ) ) ;
#3600 = ADVANCED_FACE ( 'NONE', ( #4943 ), #5180, .T. ) ;
#3601 = CARTESIAN_POINT ( 'NONE',  ( 0.000000000000000000, 71.01020514433645303, -0.5000000000000000000 ) ) ;
#3602 = CARTESIAN_POINT ( 'NONE',  ( -41.00000000000000000, -4.286263797015736496E-15, 8.499999999999998224 ) ) ;
#3603 = DIRECTION ( 'NONE',  ( 1.000000000000000000, 0.000000000000000000, -0.000000000000000000 ) ) ;
#3604 = CARTESIAN_POINT ( 'NONE',  ( -40.79557129359547929, 100.6404192164769000, -0.7730400384045151840 ) ) ;
#3605 = CARTESIAN_POINT ( 'NONE',  ( 55.99165482216006495, 2.525950835318804266, -2.499999999999997335 ) ) ;
#3606 = CIRCLE ( 'NONE', #10994, 77.49999999999998579 ) ;
#3607 = CARTESIAN_POINT ( 'NONE',  ( -10.00000000000000711, 140.0000000000000000, -2.500000000000000000 ) ) ;
#3608 = AXIS2_PLACEMENT_3D ( 'NONE', #3512, #3379, #11022 ) ;
#3609 = CARTESIAN_POINT ( 'NONE',  ( -10.69346802281034847, -6.949821576306442594, -2.606381880848196280E-15 ) ) ;
#3610 = EDGE_CURVE ( 'NONE', #10241, #12162, #1651, .T. ) ;
#3611 = CARTESIAN_POINT ( 'NONE',  ( -10.69381717166375800, 53.83378072214353693, -2.739695864762105467E-15 ) ) ;
#3612 = ORIENTED_EDGE ( 'NONE', *, *, #3506, .F. ) ;
#3613 = DIRECTION ( 'NONE',  ( 0.000000000000000000, 0.000000000000000000, 1.000000000000000000 ) ) ;
#3614 = EDGE_CURVE ( 'NONE', #2577, #2559, #3889, .T. ) ;
#3615 = ORIENTED_EDGE ( 'NONE', *, *, #452, .F. ) ;
#3616 = EDGE_CURVE ( 'NONE', #11767, #5587, #8324, .T. ) ;
#3617 = LINE ( 'NONE', #10079, #9280 ) ;
#3618 = APPLICATION_PROTOCOL_DEFINITION ( 'draft international standard', 'automotive_design', 1998, #10764 ) ;
#3619 = ORIENTED_EDGE ( 'NONE', *, *, #11052, .F. ) ;
#3620 = CARTESIAN_POINT ( 'NONE',  ( 21.34086416022640265, 21.53318388236929692, 5.637851296924623057E-15 ) ) ;
#3621 = CARTESIAN_POINT ( 'NONE',  ( -39.42692690461824157, 101.2627928944373963, 2.396630853396260807 ) ) ;
#3622 = CARTESIAN_POINT ( 'NONE',  ( -35.00000000000000000, -4.286263797015736496E-15, -7.500000000000000000 ) ) ;
#3623 = PRODUCT_DEFINITION_CONTEXT ( 'detailed design', #4587, 'design' ) ;
#3624 = CARTESIAN_POINT ( 'NONE',  ( 4.259889153847074894, -78.36053266853434707, 9.185913434196624650 ) ) ;
#3625 = VERTEX_POINT ( 'NONE', #10344 ) ;
#3626 = VECTOR ( 'NONE', #9741, 1000.000000000000000 ) ;
#3627 = VERTEX_POINT ( 'NONE', #11460 ) ;
#3628 = ADVANCED_FACE ( 'NONE', ( #9017, #13324 ), #7110, .F. ) ;
#3629 = CYLINDRICAL_SURFACE ( 'NONE', #12358, 12.49999999999999289 ) ;
#3630 = EDGE_CURVE ( 'NONE', #769, #7675, #7862, .T. ) ;
#3631 = ORIENTED_EDGE ( 'NONE', *, *, #6026, .T. ) ;
#3632 = DIRECTION ( 'NONE',  ( 0.000000000000000000, 1.000000000000000000, 0.000000000000000000 ) ) ;
#3633 = DIRECTION ( 'NONE',  ( -2.797435172181481150E-17, 1.000000000000000000, -1.765856845898762549E-18 ) ) ;
#3634 = CARTESIAN_POINT ( 'NONE',  ( -9.661733384749148001, -70.21865067344228351, -3.001891213421562732 ) ) ;
#3635 = CARTESIAN_POINT ( 'NONE',  ( -34.27497211191902693, 108.1406786207261916, 0.9834270823685512530 ) ) ;
#3636 = CARTESIAN_POINT ( 'NONE',  ( 7.721449841176848849, -88.91797570967655417, -4.656840822883729913 ) ) ;
#3637 = CARTESIAN_POINT ( 'NONE',  ( 10.69381717166375445, 16.13466892210585613, 1.286493866206055931E-15 ) ) ;
#3638 = VERTEX_POINT ( 'NONE', #3958 ) ;
#3639 = VECTOR ( 'NONE', #1251, 1000.000000000000000 ) ;
#3640 = ORIENTED_EDGE ( 'NONE', *, *, #4741, .T. ) ;
#3641 = VERTEX_POINT ( 'NONE', #6980 ) ;
#3642 = VECTOR ( 'NONE', #6161, 1000.000000000000000 ) ;
#3643 = CIRCLE ( 'NONE', #13347, 15.29705854078138749 ) ;
#3644 = ORIENTED_EDGE ( 'NONE', *, *, #7132, .T. ) ;
#3645 = DIRECTION ( 'NONE',  ( 0.000000000000000000, -1.000000000000000000, 2.775557561562888984E-15 ) ) ;
#3646 = CIRCLE ( 'NONE', #7676, 9.000000000008999024 ) ;
#3647 = CARTESIAN_POINT ( 'NONE',  ( -7.612107525059103041E-16, 27.21102387199583816, -4.805077278827845308E-17 ) ) ;
#3648 = EDGE_LOOP ( 'NONE', ( #5995, #2786, #2881, #9372 ) ) ;
#3649 = DIRECTION ( 'NONE',  ( -2.797435172181481150E-17, 1.000000000000000000, -1.765856845898762549E-18 ) ) ;
#3650 = DIRECTION ( 'NONE',  ( -6.158143864569485777E-17, -2.736152283717910599E-16, 1.000000000000000000 ) ) ;
#3651 = AXIS2_PLACEMENT_3D ( 'NONE', #9676, #7636, #11845 ) ;
#3652 = CARTESIAN_POINT ( 'NONE',  ( -1.423465862495650436, -128.7272727272635962, 3.918423281947951864 ) ) ;
#3653 = DIRECTION ( 'NONE',  ( -6.158143864569485777E-17, -2.736152283717910599E-16, 1.000000000000000000 ) ) ;
#3654 = CARTESIAN_POINT ( 'NONE',  ( -8.385254915620294014, 12.70483462268159869, -2.243491919447391838E-17 ) ) ;
#3655 = CARTESIAN_POINT ( 'NONE',  ( 0.5078243831711967138, -154.2164502166737066, 1.847253022829126623 ) ) ;
#3656 = DIRECTION ( 'NONE',  ( -2.797435172181481150E-17, 1.000000000000000000, -1.765856845898762549E-18 ) ) ;
#3657 = CARTESIAN_POINT ( 'NONE',  ( -10.69346802281034492, 21.32451227372186864, -1.384884210559934224E-15 ) ) ;
#3658 = DIRECTION ( 'NONE',  ( -1.224646799147353207E-16, 1.000000000000000000, -0.000000000000000000 ) ) ;
#3659 = ORIENTED_EDGE ( 'NONE', *, *, #10287, .T. ) ;
#3660 = ORIENTED_EDGE ( 'NONE', *, *, #3858, .T. ) ;
#3661 = VERTEX_POINT ( 'NONE', #9290 ) ;
#3662 = CARTESIAN_POINT ( 'NONE',  ( 1.823996912523629943, -150.1972678403818122, -0.6830470970659942020 ) ) ;
#3663 = VERTEX_POINT ( 'NONE', #11260 ) ;
#3664 = CIRCLE ( 'NONE', #5447, 9.000000000008999024 ) ;
#3665 = CARTESIAN_POINT ( 'NONE',  ( -0.4120236738796625442, -101.0325188118372068, -7.520994285903035426 ) ) ;
#3666 = CARTESIAN_POINT ( 'NONE',  ( 10.00024727050385920, -5.026167870790865244, -2.602085213965210642E-15 ) ) ;
#3667 = VECTOR ( 'NONE', #6996, 1000.000000000000000 ) ;
#3668 = DIRECTION ( 'NONE',  ( -0.8735848310779960046, 0.4866719047884612293, 9.637352644305955116E-17 ) ) ;
#3669 = CARTESIAN_POINT ( 'NONE',  ( -2.517691654963332357E-15, 90.00000000000000000, -1.589271161308885878E-16 ) ) ;
#3670 = ORIENTED_EDGE ( 'NONE', *, *, #7148, .T. ) ;
#3671 = ORIENTED_EDGE ( 'NONE', *, *, #11334, .T. ) ;
#3672 = DIRECTION ( 'NONE',  ( -2.797435172181481150E-17, 1.000000000000000000, -1.765856845898762549E-18 ) ) ;
#3673 = CARTESIAN_POINT ( 'NONE',  ( -0.8895390116475855313, -145.6397668398474821, 2.172994011171002882 ) ) ;
#3674 = CARTESIAN_POINT ( 'NONE',  ( 4.367873154833908700, 91.47215508561177444, -2.433639722925613924 ) ) ;
#3675 = DIRECTION ( 'NONE',  ( 0.000000000000000000, 0.000000000000000000, 1.000000000000000000 ) ) ;
#3676 = DIRECTION ( 'NONE',  ( 1.000000000000000000, 0.000000000000000000, 0.000000000000000000 ) ) ;
#3677 = EDGE_CURVE ( 'NONE', #6892, #11850, #8531, .T. ) ;
#3678 = CARTESIAN_POINT ( 'NONE',  ( -39.10039359579069895, 101.4951258812516954, -2.486679384192856723 ) ) ;
#3679 = CARTESIAN_POINT ( 'NONE',  ( -28.79177319725820894, -26.24642857144861807, 4.000000000000000000 ) ) ;
#3680 = EDGE_CURVE ( 'NONE', #2958, #2969, #10254, .T. ) ;
#3681 = CARTESIAN_POINT ( 'NONE',  ( 10.69346802281034847, -25.79937747632526879, 0.000000000000000000 ) ) ;
#3682 = CARTESIAN_POINT ( 'NONE',  ( -8.385254915620292238, 15.32944684068712782, -1.081036776539837060E-15 ) ) ;
#3683 = AXIS2_PLACEMENT_3D ( 'NONE', #1179, #9726, #8807 ) ;
#3684 = ORIENTED_EDGE ( 'NONE', *, *, #12975, .T. ) ;
#3685 = CARTESIAN_POINT ( 'NONE',  ( 3.917571877187554286, 90.55481622686230025, 3.109379165354180685 ) ) ;
#3686 = VERTEX_POINT ( 'NONE', #7177 ) ;
#3687 = CARTESIAN_POINT ( 'NONE',  ( 4.481549107982976565, -153.6493506492915628, -1.751282401325547022 ) ) ;
#3688 = CIRCLE ( 'NONE', #5947, 8.385254915620292238 ) ;
#3689 = ORIENTED_EDGE ( 'NONE', *, *, #969, .F. ) ;
#3690 = CARTESIAN_POINT ( 'NONE',  ( -10.00000000000000000, 98.00000000000000000, -2.500000000000000000 ) ) ;
#3691 = SHAPE_DEFINITION_REPRESENTATION ( #13049, #3787 ) ;
#3692 = CARTESIAN_POINT ( 'NONE',  ( -12.02287503513836775, -157.8181818181456322, 0.9430477860708889049 ) ) ;
#3693 = EDGE_CURVE ( 'NONE', #4918, #5054, #13525, .T. ) ;
#3694 = DIRECTION ( 'NONE',  ( -2.797435172181481150E-17, 1.000000000000000000, -1.765856845898762549E-18 ) ) ;
#3695 = CARTESIAN_POINT ( 'NONE',  ( -39.95750226049207043, 100.9609979968138589, 2.096206072712051061 ) ) ;
#3696 = AXIS2_PLACEMENT_3D ( 'NONE', #12146, #6813, #11088 ) ;
#3697 = ADVANCED_FACE ( 'NONE', ( #10469 ), #3168, .T. ) ;
#3698 = CARTESIAN_POINT ( 'NONE',  ( -10.69346802281034492, 21.32451227372186864, -1.384884210559934224E-15 ) ) ;
#3699 = CARTESIAN_POINT ( 'NONE',  ( -14.13596196814457784, -39.17949320881311337, 28.27192393628914502 ) ) ;
#3700 = STYLED_ITEM ( 'NONE', ( #11925 ), #7406 ) ;
#3701 = EDGE_CURVE ( 'NONE', #5708, #1662, #12824, .T. ) ;
#3702 = EDGE_CURVE ( 'NONE', #2835, #11415, #5387, .T. ) ;
#3703 = VERTEX_POINT ( 'NONE', #10605 ) ;
#3704 = CARTESIAN_POINT ( 'NONE',  ( 32.05482125692310547, -25.32934902781011743, 2.499999999999992895 ) ) ;
#3705 = CIRCLE ( 'NONE', #4602, 5.000000000000000888 ) ;
#3706 = EDGE_LOOP ( 'NONE', ( #12113, #13753, #4595, #7319 ) ) ;
#3707 = FACE_OUTER_BOUND ( 'NONE', #489, .T. ) ;
#3708 = AXIS2_PLACEMENT_3D ( 'NONE', #5262, #10397, #7097 ) ;
#3709 = DIRECTION ( 'NONE',  ( -1.000000000000000000, 0.000000000000000000, 0.000000000000000000 ) ) ;
#3710 = EDGE_CURVE ( 'NONE', #5877, #575, #4969, .T. ) ;
#3711 = DIRECTION ( 'NONE',  ( 1.000000000000000000, 0.000000000000000000, 0.000000000000000000 ) ) ;
#3712 = LINE ( 'NONE', #7846, #11108 ) ;
#3713 = CARTESIAN_POINT ( 'NONE',  ( 0.1370278527897716703, -81.54378588852601695, -9.869404650674356461 ) ) ;
#3714 = B_SPLINE_CURVE_WITH_KNOTS ( 'NONE', 3,
 ( #8484, #12457, #8426, #7300 ),
 .UNSPECIFIED., .F., .F.,
 ( 4, 4 ),
 ( 0.000000000000000000, 1.000000000000000000 ),
 .UNSPECIFIED. ) ;
#3715 = CARTESIAN_POINT ( 'NONE',  ( -10.69381717166375623, -30.98922082794128485, -21.38763434332751956 ) ) ;
#3716 = AXIS2_PLACEMENT_3D ( 'NONE', #5194, #8286, #12583 ) ;
#3717 = ORIENTED_EDGE ( 'NONE', *, *, #8736, .F. ) ;
#3718 = EDGE_CURVE ( 'NONE', #10192, #357, #1070, .T. ) ;
#3719 = VERTEX_POINT ( 'NONE', #7312 ) ;
#3720 = COLOUR_RGB ( '', 0.31764706, 0.68627451, 0.89019608) ;
#3721 = ORIENTED_EDGE ( 'NONE', *, *, #2749, .T. ) ;
#3722 = EDGE_CURVE ( 'NONE', #12269, #5851, #6468, .T. ) ;
#3723 = ORIENTED_EDGE ( 'NONE', *, *, #8755, .T. ) ;
#3724 = CYLINDRICAL_SURFACE ( 'NONE', #2216, 2.500000000000002220 ) ;
#3725 = CARTESIAN_POINT ( 'NONE',  ( -2.224254061606479205, -80.66666666666665719, 9.925145656127780214 ) ) ;
#3726 = ORIENTED_EDGE ( 'NONE', *, *, #7911, .T. ) ;
#3727 = CARTESIAN_POINT ( 'NONE',  ( 13.76342357120274862, 14.11587126553561689, 3.035766082959412415E-15 ) ) ;
#3728 = DIRECTION ( 'NONE',  ( -1.000000000000000000, 0.000000000000000000, 0.000000000000000000 ) ) ;
#3729 = B_SPLINE_CURVE_WITH_KNOTS ( 'NONE', 3,
 ( #9231, #7049, #7114, #8109 ),
 .UNSPECIFIED., .F., .F.,
 ( 4, 4 ),
 ( 0.000000000000000000, 1.000000000000000000 ),
 .UNSPECIFIED. ) ;
#3730 = CARTESIAN_POINT ( 'NONE',  ( 6.459897978785722472, -117.0909090909104435, 0.7661034210344527251 ) ) ;
#3731 = CARTESIAN_POINT ( 'NONE',  ( 12.99579180576516002, 45.23395377697383424, 25.99158361153033070 ) ) ;
#3732 = DIRECTION ( 'NONE',  ( -1.000000000000000000, 0.000000000000000000, 0.000000000000000000 ) ) ;
#3733 = CARTESIAN_POINT ( 'NONE',  ( 1.995220113909527360, -142.5800865799446058, 1.459423439933475564 ) ) ;
#3734 = CYLINDRICAL_SURFACE ( 'NONE', #10851, 50.00000000000001421 ) ;
#3735 = CARTESIAN_POINT ( 'NONE',  ( 15.34998809918498353, -16.25417180422370933, -3.363251165709652213 ) ) ;
#3736 = DIRECTION ( 'NONE',  ( -6.158143864569485777E-17, -2.736152283717910599E-16, 1.000000000000000000 ) ) ;
#3737 = VERTEX_POINT ( 'NONE', #7445 ) ;
#3738 = ORIENTED_EDGE ( 'NONE', *, *, #2009, .T. ) ;
#3739 = CIRCLE ( 'NONE', #12256, 14.99999999999999112 ) ;
#3740 = CARTESIAN_POINT ( 'NONE',  ( 1.669761519840590847, -153.2741505684571166, 0.4353783135838689700 ) ) ;
#3741 = VERTEX_POINT ( 'NONE', #871 ) ;
#3742 = CARTESIAN_POINT ( 'NONE',  ( 0.1741682660668757709, -122.8707046542772616, 4.915355393405350881 ) ) ;
#3743 = CARTESIAN_POINT ( 'NONE',  ( -60.00000000000001421, -4.286263797015736496E-15, 7.500000000000000000 ) ) ;
#3744 = CARTESIAN_POINT ( 'NONE',  ( 0.000000000000000000, 71.01020514433645303, 2.500000000000000000 ) ) ;
#3745 = ORIENTED_EDGE ( 'NONE', *, *, #5359, .T. ) ;
#3746 = ORIENTED_EDGE ( 'NONE', *, *, #8431, .F. ) ;
#3747 = DIRECTION ( 'NONE',  ( 0.000000000000000000, 0.000000000000000000, 1.000000000000000000 ) ) ;
#3748 = VERTEX_POINT ( 'NONE', #9494 ) ;
#3749 = DIRECTION ( 'NONE',  ( -0.000000000000000000, -0.000000000000000000, -1.000000000000000000 ) ) ;
#3750 = DIRECTION ( 'NONE',  ( 0.000000000000000000, 0.000000000000000000, 1.000000000000000000 ) ) ;
#3751 = CARTESIAN_POINT ( 'NONE',  ( -25.00000000000000355, 120.0000000000000142, -7.500000000000000000 ) ) ;
#3752 = PLANE ( 'NONE',  #9792 ) ;
#3753 = CARTESIAN_POINT ( 'NONE',  ( -2.517691654963332357E-15, 90.00000000000000000, -1.589271161308885878E-16 ) ) ;
#3754 = DIRECTION ( 'NONE',  ( 0.6000000000000001998, -0.7999999999999999334, 0.000000000000000000 ) ) ;
#3755 = ORIENTED_EDGE ( 'NONE', *, *, #13436, .F. ) ;
#3756 = FACE_OUTER_BOUND ( 'NONE', #12279, .T. ) ;
#3757 = EDGE_LOOP ( 'NONE', ( #7015, #63, #6672, #9246 ) ) ;
#3758 = CARTESIAN_POINT ( 'NONE',  ( -8.723672207955784685, -129.7272727272731743, 9.720751085824094417 ) ) ;
#3759 = EDGE_LOOP ( 'NONE', ( #13531, #13895, #13897, #3293 ) ) ;
#3760 = ORIENTED_EDGE ( 'NONE', *, *, #4741, .F. ) ;
#3761 = FACE_OUTER_BOUND ( 'NONE', #2918, .T. ) ;
#3762 =( BOUNDED_SURFACE ( )  B_SPLINE_SURFACE ( 3, 3, ( 
 ( #7597, #120, #1095, #1231 ),
 ( #9847, #11947, #11745, #2200 ),
 ( #11880, #13024, #2406, #9645 ),
 ( #8791, #6488, #2133, #4307 ) ),
 .UNSPECIFIED., .F., .F., .T. ) 
 B_SPLINE_SURFACE_WITH_KNOTS ( ( 4, 4 ),
 ( 4, 4 ),
 ( 0.000000000000000000, 1.000000000000000000 ),
 ( 0.000000000000000000, 1.000000000000000000 ),
 .UNSPECIFIED. ) 
 GEOMETRIC_REPRESENTATION_ITEM ( )  RATIONAL_B_SPLINE_SURFACE ( (
 ( 1.000000000000000000, 0.3333333333333334259, 0.3333333333333334259, 1.000000000000000000),
 ( 1.000000000000000000, 0.3333333333333334259, 0.3333333333333334259, 1.000000000000000000),
 ( 1.000000000000000000, 0.3333333333333334259, 0.3333333333333334259, 1.000000000000000000),
 ( 1.000000000000000000, 0.3333333333333334259, 0.3333333333333334259, 1.000000000000000000) ) ) 
 REPRESENTATION_ITEM ( '' )  SURFACE ( )  );
#3763 = LINE ( 'NONE', #8046, #6821 ) ;
#3764 = DIRECTION ( 'NONE',  ( -1.000000000000000000, 0.000000000000000000, 0.000000000000000000 ) ) ;
#3765 = CARTESIAN_POINT ( 'NONE',  ( 15.29705854078139282, 36.63580182200524149, -30.59411708156277854 ) ) ;
#3766 = DIRECTION ( 'NONE',  ( -2.797435172181481150E-17, 1.000000000000000000, -1.765856845898762549E-18 ) ) ;
#3767 = CARTESIAN_POINT ( 'NONE',  ( -10.69346802281034847, -35.22415542633469698, 21.38693604562069339 ) ) ;
#3768 = CARTESIAN_POINT ( 'NONE',  ( 2.595030052768164897, -79.59366867652133237, 9.795566994422893359 ) ) ;
#3769 = VERTEX_POINT ( 'NONE', #7244 ) ;
#3770 = AXIS2_PLACEMENT_3D ( 'NONE', #11498, #9468, #8406 ) ;
#3771 = ORIENTED_EDGE ( 'NONE', *, *, #8007, .F. ) ;
#3772 = TOROIDAL_SURFACE ( 'NONE', #11379, 72.49999999999998579, 5.000000000000000000 ) ;
#3773 = EDGE_CURVE ( 'NONE', #11361, #1587, #10115, .T. ) ;
#3774 = CARTESIAN_POINT ( 'NONE',  ( 8.385254915620297567, -24.99427717735608567, -16.77050983124058803 ) ) ;
#3775 = EDGE_CURVE ( 'NONE', #12375, #7235, #1375, .T. ) ;
#3776 = ADVANCED_FACE ( 'NONE', ( #1986 ), #9232, .T. ) ;
#3777 = EDGE_LOOP ( 'NONE', ( #12951, #8664, #12764, #13721 ) ) ;
#3778 = ADVANCED_FACE ( 'NONE', ( #6402 ), #5640, .T. ) ;
#3779 = DIRECTION ( 'NONE',  ( -1.224646799147353207E-16, 1.000000000000000000, -0.000000000000000000 ) ) ;
#3780 = EDGE_CURVE ( 'NONE', #11568, #1753, #8542, .T. ) ;
#3781 = AXIS2_PLACEMENT_3D ( 'NONE', #3843, #8124, #12408 ) ;
#3782 = CARTESIAN_POINT ( 'NONE',  ( -10.69346802281035558, 77.87317997377837742, 21.38693604562069694 ) ) ;
#3783 = CARTESIAN_POINT ( 'NONE',  ( -9.243399937414574552, -71.03723845604672249, -4.118320465786138307 ) ) ;
#3784 = DIRECTION ( 'NONE',  ( 0.000000000000000000, -0.000000000000000000, 1.000000000000000000 ) ) ;
#3785 = CARTESIAN_POINT ( 'NONE',  ( 7.116416985698259090, -87.92852090411608401, -5.737785015158151758 ) ) ;
#3786 = CARTESIAN_POINT ( 'NONE',  ( 12.99579180576516357, 16.95961992694555676, 1.563427368938892079E-15 ) ) ;
#3787 = SHAPE_REPRESENTATION ( 'Pivot Axle Pins', ( #8193 ), #13606 ) ;
#3788 = ORIENTED_EDGE ( 'NONE', *, *, #7724, .T. ) ;
#3789 = AXIS2_PLACEMENT_3D ( 'NONE', #12515, #2899, #2971 ) ;
#3790 = DIRECTION ( 'NONE',  ( -2.797435172181481150E-17, 1.000000000000000000, -1.765856845898762549E-18 ) ) ;
#3791 = AXIS2_PLACEMENT_3D ( 'NONE', #5276, #8304, #943 ) ;
#3792 = CARTESIAN_POINT ( 'NONE',  ( 1.376272962219654117, -80.66666666666658614, 10.07778225401747996 ) ) ;
#3793 = ORIENTED_EDGE ( 'NONE', *, *, #5211, .T. ) ;
#3794 = CARTESIAN_POINT ( 'NONE',  ( 8.043602938545538095, -72.64880123058061656, 6.161478615796911029 ) ) ;
#3795 = EDGE_CURVE ( 'NONE', #8398, #11958, #5477, .T. ) ;
#3796 = CARTESIAN_POINT ( 'NONE',  ( 6.267146549263187261, -111.2727272727290142, -1.834821170859801009 ) ) ;
#3797 = DIRECTION ( 'NONE',  ( -6.158143864569485777E-17, -2.736152283717910599E-16, 1.000000000000000000 ) ) ;
#3798 = CARTESIAN_POINT ( 'NONE',  ( -12.99553232110413958, 11.07475474455194053, -1.630606568990249473E-15 ) ) ;
#3799 = CARTESIAN_POINT ( 'NONE',  ( 4.114679947050920994, -133.0909090909029260, 0.08888163046386921007 ) ) ;
#3800 = CYLINDRICAL_SURFACE ( 'NONE', #1246, 25.50000000002549783 ) ;
#3801 = DIRECTION ( 'NONE',  ( 1.000000000000000000, 0.000000000000000000, 0.000000000000000000 ) ) ;
#3802 = VERTEX_POINT ( 'NONE', #6815 ) ;
#3803 = AXIS2_PLACEMENT_3D ( 'NONE', #9143, #8025, #1566 ) ;
#3804 = EDGE_LOOP ( 'NONE', ( #12164, #8864, #1831, #5664 ) ) ;
#3805 = CARTESIAN_POINT ( 'NONE',  ( -9.561354441693807661E-16, 34.17900274070598243, -6.035522597566817733E-17 ) ) ;
#3806 = VERTEX_POINT ( 'NONE', #7579 ) ;
#3807 = CARTESIAN_POINT ( 'NONE',  ( 4.962868326705308419, -115.9843930091672632, 2.901736775568028559 ) ) ;
#3808 = DIRECTION ( 'NONE',  ( -1.000000000000000000, 0.000000000000000000, 0.000000000000000000 ) ) ;
#3809 = EDGE_CURVE ( 'NONE', #5305, #11568, #10766, .T. ) ;
#3810 = CARTESIAN_POINT ( 'NONE',  ( -39.06230589874905235, 109.5835921350012683, 2.499999999999999556 ) ) ;
#3811 = CIRCLE ( 'NONE', #11644, 15.70031846811053455 ) ;
#3812 = CARTESIAN_POINT ( 'NONE',  ( 16.29599561779310335, 1.298160649189404880, -2.500000000000000000 ) ) ;
#3813 = ORIENTED_EDGE ( 'NONE', *, *, #12940, .F. ) ;
#3814 = EDGE_LOOP ( 'NONE', ( #7084, #8044, #11437, #8241, #10446, #13818, #12377, #5021, #1732, #7436, #817, #602 ) ) ;
#3815 = CARTESIAN_POINT ( 'NONE',  ( 34.24999999999975842, -135.0000000000000000, 0.000000000000000000 ) ) ;
#3816 = CARTESIAN_POINT ( 'NONE',  ( 3.290186468814228160, -129.2036444113705613, -2.543516287984220359 ) ) ;
#3817 = EDGE_CURVE ( 'NONE', #3719, #12589, #2554, .T. ) ;
#3818 = CIRCLE ( 'NONE', #2931, 14.99999999999998934 ) ;
#3819 = CIRCLE ( 'NONE', #10528, 9.000000000008999024 ) ;
#3820 = DIRECTION ( 'NONE',  ( -0.000000000000000000, -0.000000000000000000, -1.000000000000000000 ) ) ;
#3821 = LINE ( 'NONE', #12450, #9888 ) ;
#3822 = DIRECTION ( 'NONE',  ( 0.000000000000000000, 0.000000000000000000, 1.000000000000000000 ) ) ;
#3823 = CARTESIAN_POINT ( 'NONE',  ( -32.50000000000000000, 110.0000000000000142, 2.499999999999999556 ) ) ;
#3824 = CARTESIAN_POINT ( 'NONE',  ( 37.49999999999999289, 120.0000000000000142, -2.499999999999998668 ) ) ;
#3825 = DIRECTION ( 'NONE',  ( 0.9960067511297463483, -0.08927794634716618161, 4.818676322152979407E-17 ) ) ;
#3826 = CIRCLE ( 'NONE', #491, 24.99999999999998934 ) ;
#3827 = ORIENTED_EDGE ( 'NONE', *, *, #2226, .F. ) ;
#3828 = AXIS2_PLACEMENT_3D ( 'NONE', #7881, #2269, #13168 ) ;
#3829 = ORIENTED_EDGE ( 'NONE', *, *, #5734, .F. ) ;
#3830 = CARTESIAN_POINT ( 'NONE',  ( -2.139171520327136644, -164.3636363670092635, -0.7092570210252939766 ) ) ;
#3831 = ORIENTED_EDGE ( 'NONE', *, *, #723, .F. ) ;
#3832 = VERTEX_POINT ( 'NONE', #1272 ) ;
#3833 = CARTESIAN_POINT ( 'NONE',  ( -1.288514859053046853E-15, 46.06057977201469100, -8.133639011647813827E-17 ) ) ;
#3834 = DIRECTION ( 'NONE',  ( 0.000000000000000000, 0.000000000000000000, 1.000000000000000000 ) ) ;
#3835 = AXIS2_PLACEMENT_3D ( 'NONE', #104, #6604, #11866 ) ;
#3836 = CARTESIAN_POINT ( 'NONE',  ( -11.18807966363002215, -153.6493506493714563, 7.768796162323401866 ) ) ;
#3837 = CIRCLE ( 'NONE', #11670, 2.000000000000000000 ) ;
#3838 = AXIS2_PLACEMENT_3D ( 'NONE', #11485, #2800, #8126 ) ;
#3839 = CARTESIAN_POINT ( 'NONE',  ( 34.99999999999999289, 25.00000000000002132, -4.000000000000000000 ) ) ;
#3840 = CARTESIAN_POINT ( 'NONE',  ( -40.56568360645884752, 100.7114851384504135, 1.410085254968631796 ) ) ;
#3841 = DIRECTION ( 'NONE',  ( 0.000000000000000000, 0.000000000000000000, 1.000000000000000000 ) ) ;
#3842 = EDGE_CURVE ( 'NONE', #13800, #4918, #4350, .T. ) ;
#3843 = CARTESIAN_POINT ( 'NONE',  ( 35.22727272727273373, 140.0412797136805523, -2.499999999999999556 ) ) ;
#3844 = ORIENTED_EDGE ( 'NONE', *, *, #13336, .T. ) ;
#3845 = EDGE_LOOP ( 'NONE', ( #5982, #12717, #3479, #5302 ) ) ;
#3846 = VERTEX_POINT ( 'NONE', #5409 ) ;
#3847 = PLANE ( 'NONE',  #6740 ) ;
#3848 = CARTESIAN_POINT ( 'NONE',  ( 15.01254563088791372, -15.83514028494776760, 2.499999999999994227 ) ) ;
#3849 = CARTESIAN_POINT ( 'NONE',  ( 41.99999999999999289, 120.0000000000000284, 2.500000000000000000 ) ) ;
#3850 = LINE ( 'NONE', #8457, #7980 ) ;
#3851 = CARTESIAN_POINT ( 'NONE',  ( -0.8141822005786675254, -105.2536593339433750, 6.965733946918862607 ) ) ;
#3852 = EDGE_CURVE ( 'NONE', #2373, #12385, #4745, .T. ) ;
#3853 = CARTESIAN_POINT ( 'NONE',  ( 8.385254915620295790, -31.79444290936001138, 1.085359338644428786E-15 ) ) ;
#3854 = EDGE_CURVE ( 'NONE', #8546, #6099, #12590, .T. ) ;
#3855 = ORIENTED_EDGE ( 'NONE', *, *, #5817, .T. ) ;
#3856 = ORIENTED_EDGE ( 'NONE', *, *, #11155, .F. ) ;
#3857 = ORIENTED_EDGE ( 'NONE', *, *, #6340, .F. ) ;
#3858 = EDGE_CURVE ( 'NONE', #5091, #5381, #268, .T. ) ;
#3859 = ORIENTED_EDGE ( 'NONE', *, *, #3565, .T. ) ;
#3860 = CARTESIAN_POINT ( 'NONE',  ( -10.69346802281034670, -25.79937747632526879, -1.218456123918935934E-15 ) ) ;
#3861 = DIRECTION ( 'NONE',  ( 0.000000000000000000, 0.000000000000000000, -1.000000000000000000 ) ) ;
#3862 = ORIENTED_EDGE ( 'NONE', *, *, #12628, .T. ) ;
#3863 = CARTESIAN_POINT ( 'NONE',  ( 9.704377265864934543, -70.11112484142813628, 2.862656032674172568 ) ) ;
#3864 =( LENGTH_UNIT ( ) NAMED_UNIT ( * ) SI_UNIT ( .MILLI., .METRE. ) );
#3865 = CARTESIAN_POINT ( 'NONE',  ( -10.69381717166375623, 44.40900277213413716, -1.466454780123922280E-15 ) ) ;
#3866 =( BOUNDED_SURFACE ( )  B_SPLINE_SURFACE ( 3, 3, ( 
 ( #2328, #3178, #318, #1160 ),
 ( #1088, #4425, #11870, #1281 ),
 ( #11735, #10873, #1346, #12813 ),
 ( #9837, #8781, #13093, #5417 ) ),
 .UNSPECIFIED., .F., .F., .T. ) 
 B_SPLINE_SURFACE_WITH_KNOTS ( ( 4, 4 ),
 ( 4, 4 ),
 ( 0.000000000000000000, 1.000000000000000000 ),
 ( 0.000000000000000000, 1.000000000000000000 ),
 .UNSPECIFIED. ) 
 GEOMETRIC_REPRESENTATION_ITEM ( )  RATIONAL_B_SPLINE_SURFACE ( (
 ( 1.000000000000000000, 0.3333333333333334259, 0.3333333333333334259, 1.000000000000000000),
 ( 1.000000000000000000, 0.3333333333333334259, 0.3333333333333334259, 1.000000000000000000),
 ( 1.000000000000000000, 0.3333333333333334259, 0.3333333333333334259, 1.000000000000000000),
 ( 1.000000000000000000, 0.3333333333333334259, 0.3333333333333334259, 1.000000000000000000) ) ) 
 REPRESENTATION_ITEM ( '' )  SURFACE ( )  );
#3867 = CARTESIAN_POINT ( 'NONE',  ( 2.301581772533156212, -133.0909090909184158, -3.282526544929044832 ) ) ;
#3868 = CYLINDRICAL_SURFACE ( 'NONE', #1711, 20.00000000000001066 ) ;
#3869 = EDGE_CURVE ( 'NONE', #13685, #6795, #7715, .T. ) ;
#3870 = AXIS2_PLACEMENT_3D ( 'NONE', #909, #11625, #6306 ) ;
#3871 = DIRECTION ( 'NONE',  ( -2.797435172181481150E-17, 1.000000000000000000, -1.765856845898762549E-18 ) ) ;
#3872 = CIRCLE ( 'NONE', #2759, 15.29705854078138927 ) ;
#3873 = DIRECTION ( 'NONE',  ( -0.000000000000000000, -0.000000000000000000, -1.000000000000000000 ) ) ;
#3874 = ORIENTED_EDGE ( 'NONE', *, *, #101, .F. ) ;
#3875 = ORIENTED_EDGE ( 'NONE', *, *, #4269, .T. ) ;
#3876 = VERTEX_POINT ( 'NONE', #4638 ) ;
#3877 = CARTESIAN_POINT ( 'NONE',  ( 1.825346184638892089, -151.7272952153482493, -0.1028462948019921580 ) ) ;
#3878 = ORIENTED_EDGE ( 'NONE', *, *, #10140, .T. ) ;
#3879 = EDGE_CURVE ( 'NONE', #4054, #11500, #7791, .T. ) ;
#3880 = ADVANCED_FACE ( 'NONE', ( #3300 ), #8773, .T. ) ;
#3881 = CARTESIAN_POINT ( 'NONE',  ( -3.965212879745630747, -97.74628899555017369, -6.871886594889189404 ) ) ;
#3882 =( REPRESENTATION_RELATIONSHIP ('NONE','NONE', #9450, #5134 ) REPRESENTATION_RELATIONSHIP_WITH_TRANSFORMATION ( #9101 )SHAPE_REPRESENTATION_RELATIONSHIP( ) );
#3883 = DIRECTION ( 'NONE',  ( 0.000000000000000000, 0.000000000000000000, 1.000000000000000000 ) ) ;
#3884 = VECTOR ( 'NONE', #11911, 1000.000000000000000 ) ;
#3885 = CARTESIAN_POINT ( 'NONE',  ( 32.95454545454546036, 135.5876619995293026, -2.499999999999998668 ) ) ;
#3886 = ORIENTED_EDGE ( 'NONE', *, *, #12722, .T. ) ;
#3887 = CARTESIAN_POINT ( 'NONE',  ( 39.06230589874904524, 109.5835921350012683, -2.499999999999999556 ) ) ;
#3888 = CARTESIAN_POINT ( 'NONE',  ( 0.01149510067628621221, -159.4799678529391826, -1.513478599014171477 ) ) ;
#3889 = LINE ( 'NONE', #4873, #12124 ) ;
#3890 = CARTESIAN_POINT ( 'NONE',  ( 35.45454545454547457, 140.4866414850956460, 2.500000000000000000 ) ) ;
#3891 = CARTESIAN_POINT ( 'NONE',  ( 10.69346802281035202, 2.474956373702985601, -21.38693604562069339 ) ) ;
#3892 = CARTESIAN_POINT ( 'NONE',  ( 27.98552063842490867, -17.38741154648219833, 2.499999999999994671 ) ) ;
#3893 = CIRCLE ( 'NONE', #1420, 31.93204061526059334 ) ;
#3894 = CARTESIAN_POINT ( 'NONE',  ( 38.79999999999999716, 101.5999999999999943, -2.500000000000000000 ) ) ;
#3895 = CARTESIAN_POINT ( 'NONE',  ( 12.99579180576516890, 64.08350967699263379, 3.183050967463143379E-15 ) ) ;
#3896 = EDGE_CURVE ( 'NONE', #7690, #10314, #1760, .T. ) ;
#3897 = ORIENTED_EDGE ( 'NONE', *, *, #275, .F. ) ;
#3898 = CARTESIAN_POINT ( 'NONE',  ( 4.067971666435306943, 90.77778941963205739, 2.909847887424534374 ) ) ;
#3899 = EDGE_LOOP ( 'NONE', ( #4503, #3009, #1282, #608, #736, #13401, #1878, #3746, #8517, #1900, #4880, #3619, #12912, #8246, #10746, #10220, #2620, #10282, #8813, #2457, #13050, #7992, #12705, #10167, #1057, #4302, #353, #7502, #9330, #6528, #11066, #8691, #800, #9969, #4794, #5319, #8885, #825, #1978, #13860, #6393, #163, #4340, #3158, #4134, #11804, #7858, #5668, #3918, #13142, #5511, #13204, #6989, #8585, #10895, #10509, #10775, #8910, #9724, #13051, #10231, #3755 ) ) ;
#3900 = FACE_OUTER_BOUND ( 'NONE', #9554, .T. ) ;
#3901 = VERTEX_POINT ( 'NONE', #6540 ) ;
#3902 = VERTEX_POINT ( 'NONE', #7865 ) ;
#3903 = AXIS2_PLACEMENT_3D ( 'NONE', #11704, #490, #6 ) ;
#3904 = CARTESIAN_POINT ( 'NONE',  ( -4.545447045960951726, 90.76293396533760927, -2.092248084982493594 ) ) ;
#3905 = DIRECTION ( 'NONE',  ( 0.000000000000000000, 0.000000000000000000, 1.000000000000000000 ) ) ;
#3906 = CARTESIAN_POINT ( 'NONE',  ( 40.87368016229836343, -22.78235879061917046, -2.500000000000003109 ) ) ;
#3907 = B_SPLINE_CURVE_WITH_KNOTS ( 'NONE', 3,
 ( #10543, #6339, #1015, #9433 ),
 .UNSPECIFIED., .F., .F.,
 ( 4, 4 ),
 ( 0.000000000000000000, 1.000000000000000000 ),
 .UNSPECIFIED. ) ;
#3908 = CARTESIAN_POINT ( 'NONE',  ( -12.99579180576517068, 7.534841976936127672, 25.99158361153032359 ) ) ;
#3909 = FACE_OUTER_BOUND ( 'NONE', #9734, .T. ) ;
#3910 = DIRECTION ( 'NONE',  ( -0.000000000000000000, -0.000000000000000000, -1.000000000000000000 ) ) ;
#3911 = CIRCLE ( 'NONE', #12882, 9.000000000009002576 ) ;
#3912 = CARTESIAN_POINT ( 'NONE',  ( -7.612107525059103041E-16, 27.21102387199583816, -4.805077278827845308E-17 ) ) ;
#3913 = AXIS2_PLACEMENT_3D ( 'NONE', #5709, #13099, #3317 ) ;
#3914 = ORIENTED_EDGE ( 'NONE', *, *, #2830, .T. ) ;
#3915 = AXIS2_PLACEMENT_3D ( 'NONE', #13488, #1792, #9306 ) ;
#3916 = B_SPLINE_CURVE_WITH_KNOTS ( 'NONE', 3,
 ( #1684, #6724, #12133, #581, #5969, #364, #10237, #2521, #4622, #10170, #4844, #11150, #8903, #4904 ),
 .UNSPECIFIED., .F., .F.,
 ( 4, 2, 2, 2, 2, 2, 4 ),
 ( 0.000000000000000000, 0.003826572935444120475, 0.005739859403166179194, 0.007653145870888239215, 0.01147971880633235665, 0.01339300527405441407, 0.01530629174177647149 ),
 .UNSPECIFIED. ) ;
#3917 = ORIENTED_EDGE ( 'NONE', *, *, #3241, .T. ) ;
#3918 = ORIENTED_EDGE ( 'NONE', *, *, #6039, .F. ) ;
#3919 = CARTESIAN_POINT ( 'NONE',  ( 10.69381717166375978, -21.56444287793185310, -21.38763434332751245 ) ) ;
#3920 = CIRCLE ( 'NONE', #11753, 15.29705854078139105 ) ;
#3921 = VECTOR ( 'NONE', #8788, 1000.000000000000000 ) ;
#3922 = CARTESIAN_POINT ( 'NONE',  ( 8.385254915620292238, -3.520109059331755219, 1.035430912652129043E-15 ) ) ;
#3923 = CARTESIAN_POINT ( 'NONE',  ( -35.45454545454546036, 140.4866414850956744, 0.5000000000000000000 ) ) ;
#3924 = CARTESIAN_POINT ( 'NONE',  ( 8.502150441026719463, -90.92014524198424397, -2.331827081617004360 ) ) ;
#3925 = CARTESIAN_POINT ( 'NONE',  ( 0.000000000000000000, -20.00000000000000355, 0.000000000000000000 ) ) ;
#3926 = ORIENTED_EDGE ( 'NONE', *, *, #5869, .T. ) ;
#3927 = ORIENTED_EDGE ( 'NONE', *, *, #10232, .T. ) ;
#3928 = VECTOR ( 'NONE', #5998, 1000.000000000000000 ) ;
#3929 = CARTESIAN_POINT ( 'NONE',  ( 15.29705854078138927, 90.00000000000000000, 1.714422261702872766E-15 ) ) ;
#3930 = CARTESIAN_POINT ( 'NONE',  ( -12.99553232110414491, -7.774801155466915858, -1.564035334333850472E-15 ) ) ;
#3931 = AXIS2_PLACEMENT_3D ( 'NONE', #5331, #10658, #6455 ) ;
#3932 = ORIENTED_EDGE ( 'NONE', *, *, #11602, .F. ) ;
#3933 = CARTESIAN_POINT ( 'NONE',  ( -4.318061424038324603, 91.66495677434029687, -2.521242278247964208 ) ) ;
#3934 = CARTESIAN_POINT ( 'NONE',  ( -25.00000000000000355, 120.0000000000000142, 2.500000000000000000 ) ) ;
#3935 = ORIENTED_EDGE ( 'NONE', *, *, #11692, .T. ) ;
#3936 = CARTESIAN_POINT ( 'NONE',  ( 26.69171018101576465, -19.44228176112429551, -2.500000000000004441 ) ) ;
#3937 =( LENGTH_UNIT ( ) NAMED_UNIT ( * ) SI_UNIT ( .MILLI., .METRE. ) );
#3938 = FACE_OUTER_BOUND ( 'NONE', #11047, .T. ) ;
#3939 = PRODUCT_DEFINITION ( 'UNKNOWN', '', #9095, #10227 ) ;
#3940 = CIRCLE ( 'NONE', #7509, 22.99999999999999645 ) ;
#3941 = DIRECTION ( 'NONE',  ( 6.158143864569485777E-17, 2.736152283717910599E-16, -1.000000000000000000 ) ) ;
#3942 = FACE_OUTER_BOUND ( 'NONE', #2937, .T. ) ;
#3943 = CARTESIAN_POINT ( 'NONE',  ( -1.158071465989066962, -149.5103943980214467, -1.626766656952254086 ) ) ;
#3944 = DIRECTION ( 'NONE',  ( 1.000000000000000000, 0.000000000000000000, 0.000000000000000000 ) ) ;
#3945 = VECTOR ( 'NONE', #12804, 1000.000000000000000 ) ;
#3946 = EDGE_LOOP ( 'NONE', ( #13145, #13172, #3349, #11716 ) ) ;
#3947 = ORIENTED_EDGE ( 'NONE', *, *, #12796, .T. ) ;
#3948 = ORIENTED_EDGE ( 'NONE', *, *, #5469, .T. ) ;
#3949 = CARTESIAN_POINT ( 'NONE',  ( 5.923806222615441541, -113.5015096987964114, 0.9909073766846139275 ) ) ;
#3950 = ADVANCED_FACE ( 'NONE', ( #13084 ), #12148, .F. ) ;
#3951 = CARTESIAN_POINT ( 'NONE',  ( -34.25812584745457201, 108.1980041606221192, 0.5000000000000000000 ) ) ;
#3952 = FACE_OUTER_BOUND ( 'NONE', #223, .T. ) ;
#3953 = ORIENTED_EDGE ( 'NONE', *, *, #571, .T. ) ;
#3954 = DIRECTION ( 'NONE',  ( -0.000000000000000000, -0.000000000000000000, -1.000000000000000000 ) ) ;
#3955 = EDGE_CURVE ( 'NONE', #3876, #7882, #8922, .T. ) ;
#3956 = FACE_OUTER_BOUND ( 'NONE', #9915, .T. ) ;
#3957 = DIRECTION ( 'NONE',  ( -6.158143864569485777E-17, -2.736152283717910599E-16, 1.000000000000000000 ) ) ;
#3958 = CARTESIAN_POINT ( 'NONE',  ( 15.29705854078139282, 8.361467971976981772, 1.856918518244840178E-15 ) ) ;
#3959 = ADVANCED_FACE ( 'NONE', ( #8700 ), #13004, .T. ) ;
#3960 = DIRECTION ( 'NONE',  ( 0.000000000000000000, -1.000000000000000000, 0.000000000000000000 ) ) ;
#3961 = ADVANCED_FACE ( 'NONE', ( #9975 ), #4496, .T. ) ;
#3962 = FACE_OUTER_BOUND ( 'NONE', #4283, .T. ) ;
#3963 = CARTESIAN_POINT ( 'NONE',  ( -19.87806660956081473, 26.74843260078020890, -2.549167750534977017 ) ) ;
#3964 = DIRECTION ( 'NONE',  ( 0.000000000000000000, 0.000000000000000000, 1.000000000000000000 ) ) ;
#3965 = DIRECTION ( 'NONE',  ( 0.000000000000000000, 0.000000000000000000, 1.000000000000000000 ) ) ;
#3966 = ORIENTED_EDGE ( 'NONE', *, *, #11903, .F. ) ;
#3967 = DIRECTION ( 'NONE',  ( 1.601283208593975514E-16, -1.000000000000000000, 0.000000000000000000 ) ) ;
#3968 = VERTEX_POINT ( 'NONE', #10935 ) ;
#3969 = CARTESIAN_POINT ( 'NONE',  ( -19.28867027886077068, -167.3636363460783798, 6.559046148772988083 ) ) ;
#3970 = ORIENTED_EDGE ( 'NONE', *, *, #13162, .F. ) ;
#3971 = VERTEX_POINT ( 'NONE', #4562 ) ;
#3972 = CARTESIAN_POINT ( 'NONE',  ( -4.961404791891401267, 89.99999999999998579, -0.6346456166747422856 ) ) ;
#3973 = FACE_OUTER_BOUND ( 'NONE', #11628, .T. ) ;
#3974 = CARTESIAN_POINT ( 'NONE',  ( 1.026257021570081918, -73.45454546207005819, 21.46608457194884068 ) ) ;
#3975 = CARTESIAN_POINT ( 'NONE',  ( 8.385254915620290461, 34.17900274070598243, -16.77050983124057737 ) ) ;
#3976 = EDGE_CURVE ( 'NONE', #2454, #3686, #2202, .T. ) ;
#3977 = CARTESIAN_POINT ( 'NONE',  ( -10.69346802281035380, 49.59884612375012836, 21.38693604562069339 ) ) ;
#3978 = CARTESIAN_POINT ( 'NONE',  ( -8.385254915620292238, 15.32944684068712782, -2.706960864746847057E-17 ) ) ;
#3979 = CARTESIAN_POINT ( 'NONE',  ( -1.410017725396658984E-15, 50.40394642271930792, -8.900615385087330109E-17 ) ) ;
#3980 = ORIENTED_EDGE ( 'NONE', *, *, #2062, .F. ) ;
#3981 = ORIENTED_EDGE ( 'NONE', *, *, #9436, .F. ) ;
#3982 = CARTESIAN_POINT ( 'NONE',  ( -10.69381717166375267, -12.13966492792242846, -21.38763434332751601 ) ) ;
#3983 = DIRECTION ( 'NONE',  ( 1.000000000000000000, 0.000000000000000000, 0.000000000000000000 ) ) ;
#3984 = EDGE_CURVE ( 'NONE', #13867, #11837, #12052, .T. ) ;
#3985 = CARTESIAN_POINT ( 'NONE',  ( 31.81818181818183433, 133.3608531424536920, -0.5000000000000000000 ) ) ;
#3986 = CARTESIAN_POINT ( 'NONE',  ( -15.29705854078139282, -1.063309978032445979, -3.758510681017264029E-15 ) ) ;
#3987 = DIRECTION ( 'NONE',  ( -2.797435172181481150E-17, 1.000000000000000000, -1.765856845898762549E-18 ) ) ;
#3988 = CARTESIAN_POINT ( 'NONE',  ( 0.1949906707164464070, -155.7802847986947654, 1.574602209766050143 ) ) ;
#3989 = CIRCLE ( 'NONE', #12284, 9.000000000009002576 ) ;
#3990 = CYLINDRICAL_SURFACE ( 'NONE', #6459, 15.29705854078139105 ) ;
#3991 = EDGE_LOOP ( 'NONE', ( #6431, #216, #13214, #2307 ) ) ;
#3992 = ORIENTED_EDGE ( 'NONE', *, *, #3854, .T. ) ;
#3993 = ORIENTED_EDGE ( 'NONE', *, *, #5211, .F. ) ;
#3994 = EDGE_LOOP ( 'NONE', ( #9587, #3999, #10983, #8139 ) ) ;
#3995 = CARTESIAN_POINT ( 'NONE',  ( -10.69381717166375800, -12.13966492792242846, -1.266741076154724095E-15 ) ) ;
#3996 = AXIS2_PLACEMENT_3D ( 'NONE', #2155, #4392, #9664 ) ;
#3997 = ORIENTED_EDGE ( 'NONE', *, *, #4608, .T. ) ;
#3998 = DIRECTION ( 'NONE',  ( 0.000000000000000000, 0.000000000000000000, 1.000000000000000000 ) ) ;
#3999 = ORIENTED_EDGE ( 'NONE', *, *, #6941, .T. ) ;
#4000 = LINE ( 'NONE', #2098, #8577 ) ;
#4001 = VECTOR ( 'NONE', #11166, 1000.000000000000114 ) ;
#4002 = CARTESIAN_POINT ( 'NONE',  ( 34.99999999999958789, 1.104930248025249758E-13, -2.499999999999999112 ) ) ;
#4003 = CARTESIAN_POINT ( 'NONE',  ( -1.146365672123090463E-15, 40.97916847270985130, -7.236334518677345233E-17 ) ) ;
#4004 = CARTESIAN_POINT ( 'NONE',  ( -6.190615655759536180E-16, 22.12961257269105531, -3.907772785857374249E-17 ) ) ;
#4005 = CARTESIAN_POINT ( 'NONE',  ( 3.905416522049567796, -121.2486883143391481, 3.232865067491931921 ) ) ;
#4006 = CYLINDRICAL_SURFACE ( 'NONE', #12909, 14.99999999999998934 ) ;
#4007 = VERTEX_POINT ( 'NONE', #2613 ) ;
#4008 = ADVANCED_FACE ( 'NONE', ( #8148 ), #6460, .T. ) ;
#4009 = ORIENTED_EDGE ( 'NONE', *, *, #5084, .T. ) ;
#4010 = ORIENTED_EDGE ( 'NONE', *, *, #8489, .T. ) ;
#4011 = CARTESIAN_POINT ( 'NONE',  ( 0.1084562595890940784, -143.6327608500317012, -2.541581260578934742 ) ) ;
#4012 = CIRCLE ( 'NONE', #2432, 20.00000000000000000 ) ;
#4013 = DIRECTION ( 'NONE',  ( -0.3926913852462017296, -0.9196703082917372374, -2.891205793291787151E-16 ) ) ;
#4014 = CARTESIAN_POINT ( 'NONE',  ( -35.00000000000000000, -4.286263797015736496E-15, 7.500000000000000000 ) ) ;
#4015 = ORIENTED_EDGE ( 'NONE', *, *, #5172, .T. ) ;
#4016 = DIRECTION ( 'NONE',  ( 2.797435172181480534E-17, -1.000000000000000000, 1.765856845898762164E-18 ) ) ;
#4017 = CARTESIAN_POINT ( 'NONE',  ( -5.728966446173876292, -108.7068931125657087, 3.285836578437095756 ) ) ;
#4018 = AXIS2_PLACEMENT_3D ( 'NONE', #9966, #649, #12283 ) ;
#4019 = CARTESIAN_POINT ( 'NONE',  ( 10.11144057928414242, -69.99977036137985920, -0.2534939170199681513 ) ) ;
#4020 = DIRECTION ( 'NONE',  ( -2.797435172181481150E-17, 1.000000000000000000, -1.765856845898762549E-18 ) ) ;
#4021 = CIRCLE ( 'NONE', #2441, 25.50000000002550138 ) ;
#4022 = DIRECTION ( 'NONE',  ( 1.000000000000000000, 0.000000000000000000, 0.000000000000000000 ) ) ;
#4023 = CARTESIAN_POINT ( 'NONE',  ( 10.69381717166375623, -2.714886977913000266, 0.000000000000000000 ) ) ;
#4024 = EDGE_CURVE ( 'NONE', #11470, #12949, #6028, .T. ) ;
#4025 = ADVANCED_FACE ( 'NONE', ( #1552 ), #9268, .T. ) ;
#4026 = DIRECTION ( 'NONE',  ( -2.797435172181481150E-17, 1.000000000000000000, -1.765856845898762549E-18 ) ) ;
#4027 = VERTEX_POINT ( 'NONE', #9203 ) ;
#4028 = AXIS2_PLACEMENT_3D ( 'NONE', #4375, #3524, #12022 ) ;
#4029 = CARTESIAN_POINT ( 'NONE',  ( 25.00000000000000355, 120.0000000000000142, -0.5000000000000000000 ) ) ;
#4030 = AXIS2_PLACEMENT_3D ( 'NONE', #6004, #674, #6981 ) ;
#4031 = ADVANCED_FACE ( 'NONE', ( #3938, #5763 ), #10117, .T. ) ;
#4032 = AXIS2_PLACEMENT_3D ( 'NONE', #8253, #6857, #2793 ) ;
#4033 = EDGE_LOOP ( 'NONE', ( #7053, #12030, #4009, #6536, #7237, #5949 ) ) ;
#4034 = AXIS2_PLACEMENT_3D ( 'NONE', #2552, #12159, #11106 ) ;
#4035 = DIRECTION ( 'NONE',  ( 0.000000000000000000, 0.000000000000000000, -1.000000000000000000 ) ) ;
#4036 = ORIENTED_EDGE ( 'NONE', *, *, #6337, .T. ) ;
#4037 = LINE ( 'NONE', #8320, #6199 ) ;
#4038 = DIRECTION ( 'NONE',  ( -0.000000000000000000, -0.000000000000000000, -1.000000000000000000 ) ) ;
#4039 = CARTESIAN_POINT ( 'NONE',  ( -2.339066459587731637E-16, 8.361467971976981772, -1.476515546007874940E-17 ) ) ;
#4040 = CARTESIAN_POINT ( 'NONE',  ( -3.722721133223385603, -134.6363636363710725, 2.741844555832380070 ) ) ;
#4041 = AXIS2_PLACEMENT_3D ( 'NONE', #1467, #2739, #434 ) ;
#4042 = CYLINDRICAL_SURFACE ( 'NONE', #4941, 15.29705854078139460 ) ;
#4043 = DIRECTION ( 'NONE',  ( -0.8735848310779960046, 0.4866719047884612293, 9.637352644305955116E-17 ) ) ;
#4044 = AXIS2_PLACEMENT_3D ( 'NONE', #7399, #6227, #6159 ) ;
#4045 = CARTESIAN_POINT ( 'NONE',  ( 10.69381717166376333, -30.98922082794128130, 0.000000000000000000 ) ) ;
#4046 = AXIS2_PLACEMENT_3D ( 'NONE', #10265, #5006, #8140 ) ;
#4047 = LINE ( 'NONE', #13632, #5798 ) ;
#4048 = ADVANCED_FACE ( 'NONE', ( #6951 ), #6887, .F. ) ;
#4049 = ORIENTED_EDGE ( 'NONE', *, *, #628, .T. ) ;
#4050 = EDGE_CURVE ( 'NONE', #13751, #5579, #10182, .T. ) ;
#4051 = EDGE_CURVE ( 'NONE', #9012, #10192, #7939, .T. ) ;
#4052 = CIRCLE ( 'NONE', #705, 5.000000000000000000 ) ;
#4053 = AXIS2_PLACEMENT_3D ( 'NONE', #3805, #1635, #4721 ) ;
#4054 = VERTEX_POINT ( 'NONE', #5839 ) ;
#4055 = DIRECTION ( 'NONE',  ( -1.000000000000000000, 0.000000000000000000, 0.000000000000000000 ) ) ;
#4056 = CARTESIAN_POINT ( 'NONE',  ( 19.06870874253413461, 13.90050210118286067, 2.500000000000003109 ) ) ;
#4057 = CARTESIAN_POINT ( 'NONE',  ( 52.27091746333575628, 18.76074118940758595, 6.505213034913026604E-15 ) ) ;
#4058 = CARTESIAN_POINT ( 'NONE',  ( 15.29705854078139282, -1.063309978032445091, 1.888916609591544936E-15 ) ) ;
#4059 = CARTESIAN_POINT ( 'NONE',  ( -0.1852015970780942489, -159.9999997928953235, 1.488522644435750886 ) ) ;
#4060 = CARTESIAN_POINT ( 'NONE',  ( -15.29705854078138749, 47.94714734142005597, -30.59411708156277854 ) ) ;
#4061 = AXIS2_PLACEMENT_3D ( 'NONE', #4660, #8947, #6838 ) ;
#4062 = ORIENTED_EDGE ( 'NONE', *, *, #2094, .F. ) ;
#4063 = EDGE_CURVE ( 'NONE', #7235, #9684, #10043, .T. ) ;
#4064 = ORIENTED_EDGE ( 'NONE', *, *, #2408, .T. ) ;
#4065 = DIRECTION ( 'NONE',  ( -1.000000000000000000, -2.797435172181480534E-17, 0.000000000000000000 ) ) ;
#4066 = ORIENTED_EDGE ( 'NONE', *, *, #11940, .T. ) ;
#4067 = VERTEX_POINT ( 'NONE', #7092 ) ;
#4068 = FACE_OUTER_BOUND ( 'NONE', #4850, .T. ) ;
#4069 = VERTEX_POINT ( 'NONE', #4788 ) ;
#4070 = CARTESIAN_POINT ( 'NONE',  ( 53.14943414785363984, 10.84564612680554241, -2.499999999999994671 ) ) ;
#4071 = CIRCLE ( 'NONE', #6533, 25.50000000002549783 ) ;
#4072 = DIRECTION ( 'NONE',  ( 1.000000000000000000, 0.000000000000000000, 0.000000000000000000 ) ) ;
#4073 = CARTESIAN_POINT ( 'NONE',  ( -13.79311422413708499, -21.62638421600851046, 7.500000000000000000 ) ) ;
#4074 = CARTESIAN_POINT ( 'NONE',  ( -60.00000000000001421, -4.286263797015736496E-15, -7.500000000000000000 ) ) ;
#4075 = CARTESIAN_POINT ( 'NONE',  ( -2.980405791994721554, -137.4311428799600492, 1.166279635936706693 ) ) ;
#4076 = CARTESIAN_POINT ( 'NONE',  ( -8.385254915620294014, 90.00000000000000000, -1.589271161308885878E-16 ) ) ;
#4077 = ORIENTED_EDGE ( 'NONE', *, *, #2119, .T. ) ;
#4078 = EDGE_LOOP ( 'NONE', ( #10109, #7156 ) ) ;
#4079 = ORIENTED_EDGE ( 'NONE', *, *, #1818, .T. ) ;
#4080 = CARTESIAN_POINT ( 'NONE',  ( -40.81228451836347659, 100.6358150620708471, 0.000000000000000000 ) ) ;
#4081 = DIRECTION ( 'NONE',  ( -6.158143864569485777E-17, -2.736152283717910599E-16, 1.000000000000000000 ) ) ;
#4082 = CIRCLE ( 'NONE', #6548, 25.50000000002549783 ) ;
#4083 = CARTESIAN_POINT ( 'NONE',  ( -6.172719407040554884, -110.2881872775037237, 1.857052143282659440 ) ) ;
#4084 = CARTESIAN_POINT ( 'NONE',  ( 13.94188849117746010, 1.893657697999893808, -2.500000000000000000 ) ) ;
#4085 = DIRECTION ( 'NONE',  ( 1.000000000000000000, 0.000000000000000000, 0.000000000000000000 ) ) ;
#4086 = AXIS2_PLACEMENT_3D ( 'NONE', #6629, #2415, #6694 ) ;
#4087 = DIRECTION ( 'NONE',  ( -6.158143864569485777E-17, -2.736152283717910599E-16, 1.000000000000000000 ) ) ;
#4088 = CARTESIAN_POINT ( 'NONE',  ( -10.69346802281034314, 2.474956373702985157, -21.38693604562069694 ) ) ;
#4089 = DIRECTION ( 'NONE',  ( -0.000000000000000000, -0.000000000000000000, -1.000000000000000000 ) ) ;
#4090 = DIRECTION ( 'NONE',  ( -0.000000000000000000, -0.000000000000000000, 1.000000000000000000 ) ) ;
#4091 = CARTESIAN_POINT ( 'NONE',  ( 24.37649275748779232, -100.0000000000000000, 7.500000000000000000 ) ) ;
#4092 = ORIENTED_EDGE ( 'NONE', *, *, #9830, .T. ) ;
#4093 = CYLINDRICAL_SURFACE ( 'NONE', #45, 9.000000000008999024 ) ;
#4094 = VECTOR ( 'NONE', #12191, 1000.000000000000000 ) ;
#4095 = LINE ( 'NONE', #4162, #9403 ) ;
#4096 = CARTESIAN_POINT ( 'NONE',  ( -8.931512003262966459, -153.6493506494496160, 10.28374512068630686 ) ) ;
#4097 = VECTOR ( 'NONE', #1269, 1000.000000000000114 ) ;
#4098 = VERTEX_POINT ( 'NONE', #8215 ) ;
#4099 = B_SPLINE_CURVE_WITH_KNOTS ( 'NONE', 3,
 ( #119, #12952, #6556, #6686 ),
 .UNSPECIFIED., .F., .F.,
 ( 4, 4 ),
 ( 0.000000000000000000, 1.000000000000000000 ),
 .UNSPECIFIED. ) ;
#4100 = CARTESIAN_POINT ( 'NONE',  ( -15.29705854078139460, -10.48808792804187284, 30.59411708156277854 ) ) ;
#4101 = ORIENTED_EDGE ( 'NONE', *, *, #7999, .F. ) ;
#4102 = CARTESIAN_POINT ( 'NONE',  ( 34.99999999999958789, 1.063887963769481123E-13, 12.50000000000000000 ) ) ;
#4103 = DIRECTION ( 'NONE',  ( -1.000000000000000000, 0.000000000000000000, 0.000000000000000000 ) ) ;
#4104 = CARTESIAN_POINT ( 'NONE',  ( 15.36839996672161668, -22.54980054760554964, 3.276782387371332650 ) ) ;
#4105 = AXIS2_PLACEMENT_3D ( 'NONE', #11575, #13724, #12499 ) ;
#4106 = CARTESIAN_POINT ( 'NONE',  ( -3.345128319330075151, -82.89610389611301855, 14.18235785815877037 ) ) ;
#4107 = FACE_OUTER_BOUND ( 'NONE', #12568, .T. ) ;
#4108 = CARTESIAN_POINT ( 'NONE',  ( -35.06230589874904524, 106.5835921350012825, -2.486789939184904430 ) ) ;
#4109 = CARTESIAN_POINT ( 'NONE',  ( 8.385254915620295790, -31.79444290936001138, 1.085359338644428786E-15 ) ) ;
#4110 = CARTESIAN_POINT ( 'NONE',  ( 11.81226048336476531, -40.00941361824966691, 23.62452096672953061 ) ) ;
#4111 = TOROIDAL_SURFACE ( 'NONE', #5445, 22.49999999999998934, 5.000000000000000000 ) ;
#4112 = ORIENTED_EDGE ( 'NONE', *, *, #11471, .F. ) ;
#4113 = AXIS2_PLACEMENT_3D ( 'NONE', #6072, #4090, #6214 ) ;
#4114 = EDGE_CURVE ( 'NONE', #2431, #6056, #13210, .T. ) ;
#4115 = EDGE_LOOP ( 'NONE', ( #3570, #162, #12231, #836, #10584, #2862, #659, #6283 ) ) ;
#4116 = DIRECTION ( 'NONE',  ( 0.000000000000000000, 1.000000000000000000, 0.000000000000000000 ) ) ;
#4117 = EDGE_CURVE ( 'NONE', #3094, #8676, #8936, .T. ) ;
#4118 = DIRECTION ( 'NONE',  ( 0.01532218268401990685, -0.9998826084685129567, -2.775705599192072226E-16 ) ) ;
#4119 = FACE_OUTER_BOUND ( 'NONE', #1071, .T. ) ;
#4120 = ADVANCED_FACE ( 'NONE', ( #5985 ), #8508, .T. ) ;
#4121 = DIRECTION ( 'NONE',  ( -1.000000000000000000, -2.081668171172168119E-15, 0.000000000000000000 ) ) ;
#4122 = EDGE_CURVE ( 'NONE', #6577, #11197, #5120, .T. ) ;
#4123 = CARTESIAN_POINT ( 'NONE',  ( -3.237931855445342677, -122.4890033182045812, -3.753960870359740465 ) ) ;
#4124 = CARTESIAN_POINT ( 'NONE',  ( -35.00000000000000000, -4.286263797015736496E-15, -7.500000000000000000 ) ) ;
#4125 = VERTEX_POINT ( 'NONE', #11512 ) ;
#4126 = ORIENTED_EDGE ( 'NONE', *, *, #5929, .T. ) ;
#4127 = AXIS2_PLACEMENT_3D ( 'NONE', #2461, #6741, #9973 ) ;
#4128 = CIRCLE ( 'NONE', #11305, 2.000000000000000000 ) ;
#4129 = CARTESIAN_POINT ( 'NONE',  ( -4.067971666435313161, 90.77778941963205739, -2.909847887424534374 ) ) ;
#4130 = EDGE_CURVE ( 'NONE', #4461, #8031, #12976, .T. ) ;
#4131 = EDGE_LOOP ( 'NONE', ( #2333, #10811, #2091, #3793 ) ) ;
#4132 = CARTESIAN_POINT ( 'NONE',  ( 15.29705854078139460, -38.76242177807012723, -30.59411708156277498 ) ) ;
#4133 = CIRCLE ( 'NONE', #9981, 25.50000000002549783 ) ;
#4134 = ORIENTED_EDGE ( 'NONE', *, *, #1401, .F. ) ;
#4135 = CARTESIAN_POINT ( 'NONE',  ( -8.385254915620297567, 31.55439052270045508, -5.572053652267360357E-17 ) ) ;
#4136 = DIRECTION ( 'NONE',  ( 1.000000000000000000, 0.000000000000000000, 0.000000000000000000 ) ) ;
#4137 = CARTESIAN_POINT ( 'NONE',  ( 8.385254915620292238, 22.12961257269105531, 9.855024866598291022E-16 ) ) ;
#4138 = EDGE_CURVE ( 'NONE', #10241, #2392, #7571, .T. ) ;
#4139 = DIRECTION ( 'NONE',  ( 1.000000000000000000, -1.734723475976808672E-15, 0.000000000000000000 ) ) ;
#4140 = CARTESIAN_POINT ( 'NONE',  ( 39.06230589874904524, 109.5835921350012683, 2.499999999999999556 ) ) ;
#4141 = CARTESIAN_POINT ( 'NONE',  ( -0.2126761085232016235, -104.1813795433902214, -7.142456545591105765 ) ) ;
#4142 = DIRECTION ( 'NONE',  ( 0.000000000000000000, 0.000000000000000000, 1.000000000000000000 ) ) ;
#4143 = AXIS2_PLACEMENT_3D ( 'NONE', #8858, #9989, #8940 ) ;
#4144 = ORIENTED_EDGE ( 'NONE', *, *, #8510, .F. ) ;
#4145 = VERTEX_POINT ( 'NONE', #9608 ) ;
#4146 = PLANE ( 'NONE',  #4243 ) ;
#4147 =( GEOMETRIC_REPRESENTATION_CONTEXT ( 3 ) GLOBAL_UNCERTAINTY_ASSIGNED_CONTEXT ( ( #10363 ) ) GLOBAL_UNIT_ASSIGNED_CONTEXT ( ( #3864, #1696, #10322 ) ) REPRESENTATION_CONTEXT ( 'NONE', 'WORKASPACE' ) );
#4148 = VERTEX_POINT ( 'NONE', #5325 ) ;
#4149 = DIRECTION ( 'NONE',  ( -1.000000000000000000, 0.000000000000000000, 0.000000000000000000 ) ) ;
#4150 = AXIS2_PLACEMENT_3D ( 'NONE', #13789, #729, #11579 ) ;
#4151 = CARTESIAN_POINT ( 'NONE',  ( -2.517691654963332357E-15, 90.00000000000000000, -1.589271161308885878E-16 ) ) ;
#4152 = CARTESIAN_POINT ( 'NONE',  ( -0.4106197315061012598, -101.8078744002022944, 7.425433182683227606 ) ) ;
#4153 = CARTESIAN_POINT ( 'NONE',  ( -1.214590548353025268, -168.0000000000001421, 1.662759693958066221 ) ) ;
#4154 = CARTESIAN_POINT ( 'NONE',  ( 8.385254915620290461, 62.45333659073423860, 9.631531405059305263E-16 ) ) ;
#4155 = PRODUCT_DEFINITION_FORMATION_WITH_SPECIFIED_SOURCE ( 'ANY', '', #9019, .NOT_KNOWN. ) ;
#4156 = CARTESIAN_POINT ( 'NONE',  ( 34.99999999999958789, 1.228057239789091624E-13, -47.50005079999998969 ) ) ;
#4157 = CIRCLE ( 'NONE', #7066, 71.99999999999998579 ) ;
#4158 = CARTESIAN_POINT ( 'NONE',  ( 12.99553232110414847, 1.649976794542512337, -25.99106464220827917 ) ) ;
#4159 = CARTESIAN_POINT ( 'NONE',  ( -8.385254915620294014, -15.56949922734665570, -9.719105456492490422E-16 ) ) ;
#4160 = ORIENTED_EDGE ( 'NONE', *, *, #7544, .T. ) ;
#4161 = LINE ( 'NONE', #2061, #2513 ) ;
#4162 = CARTESIAN_POINT ( 'NONE',  ( 30.68181818181819054, 131.1340442853780530, 7.500000000000000000 ) ) ;
#4163 = CARTESIAN_POINT ( 'NONE',  ( 3.345128319332408839, -82.89610389611962660, -14.18235785815831917 ) ) ;
#4164 = ORIENTED_EDGE ( 'NONE', *, *, #4460, .F. ) ;
#4165 = CARTESIAN_POINT ( 'NONE',  ( 10.69381717166375800, -12.13966492792242846, 2.619229793989004345E-15 ) ) ;
#4166 = ORIENTED_EDGE ( 'NONE', *, *, #6323, .F. ) ;
#4167 = CARTESIAN_POINT ( 'NONE',  ( 155.9864723944028810, -111.6214737678657087, -2.500000000000000000 ) ) ;
#4168 = DIRECTION ( 'NONE',  ( 1.000000000000000000, 0.000000000000000000, 0.000000000000000000 ) ) ;
#4169 = DIRECTION ( 'NONE',  ( 0.000000000000000000, 0.000000000000000000, 1.000000000000000000 ) ) ;
#4170 = CARTESIAN_POINT ( 'NONE',  ( 0.01432886326166990174, -82.89610389604476381, 5.147384767213183387 ) ) ;
#4171 = DIRECTION ( 'NONE',  ( -0.000000000000000000, -0.000000000000000000, -1.000000000000000000 ) ) ;
#4172 = CARTESIAN_POINT ( 'NONE',  ( 50.89489709276795537, 9.943703908052050622, 2.500000000000003997 ) ) ;
#4173 = DIRECTION ( 'NONE',  ( 0.1234677578012386562, 1.701584941912606716E-18, -0.9923485843107423543 ) ) ;
#4174 = CARTESIAN_POINT ( 'NONE',  ( 22.00707094244967621, -21.94159963418280057, -6.505213034913026604E-15 ) ) ;
#4175 = EDGE_CURVE ( 'NONE', #13094, #4673, #10040, .T. ) ;
#4176 = CIRCLE ( 'NONE', #10450, 9.000000000009002576 ) ;
#4177 = EDGE_LOOP ( 'NONE', ( #10448, #3717, #3659, #13376 ) ) ;
#4178 =( NAMED_UNIT ( * ) SI_UNIT ( $, .STERADIAN. ) SOLID_ANGLE_UNIT ( ) );
#4179 = ORIENTED_EDGE ( 'NONE', *, *, #1120, .T. ) ;
#4180 = CARTESIAN_POINT ( 'NONE',  ( -2.303009741871944172E-17, 0.8232575913728890082, -1.453755053663958216E-18 ) ) ;
#4181 = LINE ( 'NONE', #5106, #1223 ) ;
#4182 = CARTESIAN_POINT ( 'NONE',  ( -8.385254915620297567, 31.55439052270045508, -2.137983544802758185E-15 ) ) ;
#4183 = CARTESIAN_POINT ( 'NONE',  ( -18.54049621773915746, 27.07720798311999388, 7.500000000000000000 ) ) ;
#4184 = CARTESIAN_POINT ( 'NONE',  ( -1.899183197727328576, -124.6925521901340090, -4.281368322782853397 ) ) ;
#4185 = CARTESIAN_POINT ( 'NONE',  ( 60.49844721164429728, -0.2814068163155462599, 1.734723475976807094E-15 ) ) ;
#4186 = ORIENTED_EDGE ( 'NONE', *, *, #1543, .T. ) ;
#4187 = EDGE_CURVE ( 'NONE', #1478, #5877, #9380, .T. ) ;
#4188 = EDGE_CURVE ( 'NONE', #3291, #11147, #5548, .T. ) ;
#4189 = ORIENTED_EDGE ( 'NONE', *, *, #3015, .F. ) ;
#4190 = EDGE_CURVE ( 'NONE', #1478, #10661, #428, .T. ) ;
#4191 = CARTESIAN_POINT ( 'NONE',  ( -3.632360187558554721, 90.29910261214918421, -3.439149220787172556 ) ) ;
#4192 = ORIENTED_EDGE ( 'NONE', *, *, #10824, .T. ) ;
#4193 = CARTESIAN_POINT ( 'NONE',  ( -14.13596196814457429, -39.17949320881311337, -3.385655485371662251E-15 ) ) ;
#4194 = VERTEX_POINT ( 'NONE', #6384 ) ;
#4195 = CARTESIAN_POINT ( 'NONE',  ( 1.616533774874506480E-14, -132.0000000000000000, 0.000000000000000000 ) ) ;
#4196 =( BOUNDED_SURFACE ( )  B_SPLINE_SURFACE ( 3, 3, ( 
 ( #4470, #2366, #8547, #9809 ),
 ( #5323, #13061, #3285, #10910 ),
 ( #10651, #7694, #4540, #5454 ),
 ( #6650, #3350, #8819, #12849 ) ),
 .UNSPECIFIED., .F., .F., .T. ) 
 B_SPLINE_SURFACE_WITH_KNOTS ( ( 4, 4 ),
 ( 4, 4 ),
 ( 0.000000000000000000, 1.000000000000000000 ),
 ( 0.000000000000000000, 1.000000000000000000 ),
 .UNSPECIFIED. ) 
 GEOMETRIC_REPRESENTATION_ITEM ( )  RATIONAL_B_SPLINE_SURFACE ( (
 ( 1.000000000000000000, 0.3333333333333334259, 0.3333333333333334259, 1.000000000000000000),
 ( 1.000000000000000000, 0.3333333333333334259, 0.3333333333333334259, 1.000000000000000000),
 ( 1.000000000000000000, 0.3333333333333334259, 0.3333333333333334259, 1.000000000000000000),
 ( 1.000000000000000000, 0.3333333333333334259, 0.3333333333333334259, 1.000000000000000000) ) ) 
 REPRESENTATION_ITEM ( '' )  SURFACE ( )  );
#4197 = B_SPLINE_CURVE_WITH_KNOTS ( 'NONE', 3,
 ( #12316, #11037, #5713, #10960 ),
 .UNSPECIFIED., .F., .F.,
 ( 4, 4 ),
 ( 0.000000000000000000, 1.000000000000000000 ),
 .UNSPECIFIED. ) ;
#4198 = CARTESIAN_POINT ( 'NONE',  ( 75.98647239440286683, -111.6214737678657087, -2.500000000000000000 ) ) ;
#4199 = CARTESIAN_POINT ( 'NONE',  ( -3.469499288793235436, -73.45454545754009246, -20.14723442201650272 ) ) ;
#4200 = AXIS2_PLACEMENT_3D ( 'NONE', #153, #6651, #11908 ) ;
#4201 = CARTESIAN_POINT ( 'NONE',  ( -24.99999999999998934, -100.0000000000000000, 5.046127144241784990 ) ) ;
#4202 = DIRECTION ( 'NONE',  ( -0.6000000000000001998, -0.7999999999999998224, 0.000000000000000000 ) ) ;
#4203 = CARTESIAN_POINT ( 'NONE',  ( -0.1946493556060955588, -155.7833351585698267, -1.574489734363575311 ) ) ;
#4204 = DIRECTION ( 'NONE',  ( 1.000000000000000000, 0.000000000000000000, 0.000000000000000000 ) ) ;
#4205 = VERTEX_POINT ( 'NONE', #4198 ) ;
#4206 = ADVANCED_FACE ( 'NONE', ( #2961 ), #8549, .T. ) ;
#4207 = ORIENTED_EDGE ( 'NONE', *, *, #11602, .T. ) ;
#4208 = VERTEX_POINT ( 'NONE', #12851 ) ;
#4209 = AXIS2_PLACEMENT_3D ( 'NONE', #13529, #3871, #8152 ) ;
#4210 = EDGE_CURVE ( 'NONE', #7680, #3433, #9479, .T. ) ;
#4211 = AXIS2_PLACEMENT_3D ( 'NONE', #6599, #5691, #6665 ) ;
#4212 = EDGE_CURVE ( 'NONE', #2032, #11251, #3529, .T. ) ;
#4213 = CARTESIAN_POINT ( 'NONE',  ( 34.99999999999958789, 1.091249486606660213E-13, 2.500000000000000000 ) ) ;
#4214 = VERTEX_POINT ( 'NONE', #10588 ) ;
#4215 = CARTESIAN_POINT ( 'NONE',  ( -10.69346802281034670, 40.17406817374066463, -2.714638868194240665E-15 ) ) ;
#4216 = CARTESIAN_POINT ( 'NONE',  ( 8.874474818771595608, -89.41029592820135008, -1.238859673556061525 ) ) ;
#4217 = DIRECTION ( 'NONE',  ( 0.000000000000000000, -1.000000000000000000, 0.000000000000000000 ) ) ;
#4218 = CARTESIAN_POINT ( 'NONE',  ( -35.00000000000000000, -4.286263797015736496E-15, -4.000000000000000000 ) ) ;
#4219 = CARTESIAN_POINT ( 'NONE',  ( -10.17548876272777036, -70.78787878787981924, -0.6371443735352790849 ) ) ;
#4220 = AXIS2_PLACEMENT_3D ( 'NONE', #3979, #8256, #9720 ) ;
#4221 = CARTESIAN_POINT ( 'NONE',  ( 3.621248221984613947E-16, -12.94488700934118341, 2.285881734483108495E-17 ) ) ;
#4222 = CARTESIAN_POINT ( 'NONE',  ( -10.69346802281034847, 30.74929022373126841, -1.418169827888134119E-15 ) ) ;
#4223 = CIRCLE ( 'NONE', #9834, 18.74900000001875355 ) ;
#4224 = CARTESIAN_POINT ( 'NONE',  ( -30.68181818181819054, 131.1340442853780814, -2.499999999999998668 ) ) ;
#4225 = CARTESIAN_POINT ( 'NONE',  ( 25.00000000000000355, 120.0000000000000284, -2.500000000000000000 ) ) ;
#4226 = ORIENTED_EDGE ( 'NONE', *, *, #10140, .F. ) ;
#4227 = CARTESIAN_POINT ( 'NONE',  ( -4.154595973944807064, -61.00000000000002842, 0.9946518452611590178 ) ) ;
#4228 = EDGE_CURVE ( 'NONE', #7931, #1659, #13877, .T. ) ;
#4229 = ORIENTED_EDGE ( 'NONE', *, *, #6100, .F. ) ;
#4230 = DIRECTION ( 'NONE',  ( 1.000000000000000000, 0.000000000000000000, 0.000000000000000000 ) ) ;
#4231 = CIRCLE ( 'NONE', #7728, 12.49999999999999289 ) ;
#4232 = EDGE_LOOP ( 'NONE', ( #1429, #4677, #7238, #10420 ) ) ;
#4233 = DIRECTION ( 'NONE',  ( 0.000000000000000000, 0.000000000000000000, 1.000000000000000000 ) ) ;
#4234 = LINE ( 'NONE', #9509, #2798 ) ;
#4235 = VECTOR ( 'NONE', #9770, 1000.000000000000000 ) ;
#4236 = CARTESIAN_POINT ( 'NONE',  ( 12.09338464843078143, -60.99999999999997158, -0.006909782851249028461 ) ) ;
#4237 = DIRECTION ( 'NONE',  ( 1.000000000000000000, 0.000000000000000000, 0.000000000000000000 ) ) ;
#4238 = CARTESIAN_POINT ( 'NONE',  ( 8.385254915620295790, 12.70483462268160046, -16.77050983124058448 ) ) ;
#4239 = CARTESIAN_POINT ( 'NONE',  ( 34.99999999999958789, 1.091249486606660213E-13, 2.500000000000000000 ) ) ;
#4240 = CARTESIAN_POINT ( 'NONE',  ( 31.28009342530033265, 25.22721338310705264, 7.806255641895631925E-15 ) ) ;
#4241 = AXIS2_PLACEMENT_3D ( 'NONE', #7045, #2633, #13475 ) ;
#4242 = CARTESIAN_POINT ( 'NONE',  ( -25.00000000000000355, 120.0000000000000142, -0.5000000000000000000 ) ) ;
#4243 = AXIS2_PLACEMENT_3D ( 'NONE', #12719, #5508, #2283 ) ;
#4244 = CIRCLE ( 'NONE', #687, 9.000000000008999024 ) ;
#4245 = ORIENTED_EDGE ( 'NONE', *, *, #1974, .T. ) ;
#4246 = CIRCLE ( 'NONE', #3356, 15.70031846811053455 ) ;
#4247 = DIRECTION ( 'NONE',  ( 0.000000000000000000, 0.000000000000000000, 1.000000000000000000 ) ) ;
#4248 = EDGE_LOOP ( 'NONE', ( #663, #6417, #9350, #4126 ) ) ;
#4249 = CARTESIAN_POINT ( 'NONE',  ( 57.84299132690245671, 11.33347904398042871, 5.204170427930421283E-15 ) ) ;
#4250 = CYLINDRICAL_SURFACE ( 'NONE', #12200, 18.74900000001875000 ) ;
#4251 = AXIS2_PLACEMENT_3D ( 'NONE', #1098, #5357, #9648 ) ;
#4252 = AXIS2_PLACEMENT_3D ( 'NONE', #668, #11182, #467 ) ;
#4253 = CARTESIAN_POINT ( 'NONE',  ( -25.00000000000000355, 120.0000000000000284, 2.500000000000000000 ) ) ;
#4254 = SURFACE_SIDE_STYLE ('',( #4588 ) ) ;
#4255 = CARTESIAN_POINT ( 'NONE',  ( 1.160247953126058107, -149.4998025384539915, 1.626383737532501650 ) ) ;
#4256 = CARTESIAN_POINT ( 'NONE',  ( -15.29705854078138927, 10.24803554138234318, 30.59411708156276788 ) ) ;
#4257 = VERTEX_POINT ( 'NONE', #5062 ) ;
#4258 = AXIS2_PLACEMENT_3D ( 'NONE', #7449, #2120, #4022 ) ;
#4259 = ORIENTED_EDGE ( 'NONE', *, *, #6202, .T. ) ;
#4260 = CIRCLE ( 'NONE', #6298, 25.50000000002549783 ) ;
#4261 = AXIS2_PLACEMENT_3D ( 'NONE', #1861, #5089, #821 ) ;
#4262 = DIRECTION ( 'NONE',  ( -1.000000000000000000, 0.000000000000000000, 0.000000000000000000 ) ) ;
#4263 = VERTEX_POINT ( 'NONE', #13787 ) ;
#4264 = DIRECTION ( 'NONE',  ( -1.224646799147353207E-16, 1.000000000000000000, -0.000000000000000000 ) ) ;
#4265 = EDGE_LOOP ( 'NONE', ( #6517, #4426, #637, #6324 ) ) ;
#4266 = FACE_OUTER_BOUND ( 'NONE', #392, .T. ) ;
#4267 = EDGE_CURVE ( 'NONE', #7855, #10906, #1980, .T. ) ;
#4268 = CARTESIAN_POINT ( 'NONE',  ( 0.000000000000000000, 71.01020514433645303, 0.5000000000000000000 ) ) ;
#4269 = EDGE_CURVE ( 'NONE', #12738, #7898, #8422, .T. ) ;
#4270 = CARTESIAN_POINT ( 'NONE',  ( 34.99999999999958789, 1.104930248025249758E-13, -2.499999999999999112 ) ) ;
#4271 = CARTESIAN_POINT ( 'NONE',  ( -1.381416026885722292, -78.35919761624415969, -10.01283214670341160 ) ) ;
#4272 = CIRCLE ( 'NONE', #6522, 27.49999999999998579 ) ;
#4273 = CARTESIAN_POINT ( 'NONE',  ( -1.552166912326615374E-15, 55.48535772202409078, -9.797919878057798703E-17 ) ) ;
#4274 = LINE ( 'NONE', #7047, #10019 ) ;
#4275 = CIRCLE ( 'NONE', #497, 4.999999999999996447 ) ;
#4276 = CARTESIAN_POINT ( 'NONE',  ( 1.792607291163630601, -80.16257883281073759, 9.968655783465312226 ) ) ;
#4277 = DIRECTION ( 'NONE',  ( 0.000000000000000000, 0.000000000000000000, 1.000000000000000000 ) ) ;
#4278 = VERTEX_POINT ( 'NONE', #12648 ) ;
#4279 = VERTEX_POINT ( 'NONE', #7296 ) ;
#4280 = ORIENTED_EDGE ( 'NONE', *, *, #207, .T. ) ;
#4281 = B_SPLINE_SURFACE_WITH_KNOTS ( 'NONE', 3, 3, ( 
 ( #1985, #13539, #8232, #4153 ),
 ( #5140, #745, #5009, #9289 ),
 ( #12520, #13604, #2904, #11459 ),
 ( #10408, #808, #13671, #2974 ),
 ( #7243, #11527, #1919, #6208 ),
 ( #10468, #8567, #11793, #8772 ),
 ( #2183, #10934, #10670, #13083 ),
 ( #7444, #9627, #1078, #13871 ),
 ( #11725, #5476, #2114, #12870 ),
 ( #5408, #96, #8633, #5838 ),
 ( #8841, #3652, #7782, #4787 ),
 ( #9064, #11012, #13380, #13151 ),
 ( #3730, #8014, #3499, #12291 ),
 ( #2463, #2681, #3796, #12366 ),
 ( #2750, #6743, #5690, #9974 ),
 ( #385, #7091, #4990, #9478 ),
 ( #5061, #3084, #9343, #13653 ),
 ( #12579, #1903, #6190, #10456 ),
 ( #5984, #9409, #7352, #3026 ),
 ( #991, #12821, #828, #11676 ),
 ( #8322, #890, #3118, #9449 ),
 ( #7327, #1941, #5094, #10559 ),
 ( #3188, #13695, #1795, #3974 ),
 ( #6225, #13822, #9378, #10358 ) ),
 .UNSPECIFIED., .F., .F., .F.,
 ( 4, 1, 1, 1, 1, 1, 1, 1, 1, 1, 1, 1, 1, 1, 1, 1, 1, 1, 1, 1, 1, 4 ),
 ( 4, 4 ),
 ( -0.1668267180224854429, -0.1624291228870498593, -0.1587644602741868916, -0.1580315277516142758, -0.1536339326161787200, -0.1471422445591071271, -0.1404411472098719693, -0.1360435520744363858, -0.1316459569390008300, -0.1272483618035652464, -0.1228507666681296628, -0.1140555763972584957, -0.1096579812618229260, -0.1052603861263873425, -0.1008627909909517728, -0.09646519585551618925, -0.08976409850628104536, -0.08327241044920945245, -0.07887481531377388277, -0.07814188279120128089, -0.07447722017833829922, -0.07007962504290271566 ),
 ( 0.003200000000000001888, 0.006800000000000002223 ),
 .UNSPECIFIED. ) ;
#4282 = DIRECTION ( 'NONE',  ( 1.000000000000000000, 0.000000000000000000, 0.000000000000000000 ) ) ;
#4283 = EDGE_LOOP ( 'NONE', ( #3723, #6922, #3584, #899 ) ) ;
#4284 = CARTESIAN_POINT ( 'NONE',  ( 8.385254915620294014, 40.97916847270985130, 9.905219695108654260E-16 ) ) ;
#4285 = CARTESIAN_POINT ( 'NONE',  ( 7.223390746404686702, -85.44318711194655691, -6.107340895223999588 ) ) ;
#4286 = ADVANCED_FACE ( 'NONE', ( #13853, #3027 ), #12711, .T. ) ;
#4287 = DIRECTION ( 'NONE',  ( 6.158143864569485777E-17, 2.736152283717910599E-16, -1.000000000000000000 ) ) ;
#4288 = CARTESIAN_POINT ( 'NONE',  ( 39.71817523509052705, -20.60992048131556942, 2.499999999999994671 ) ) ;
#4289 = EDGE_CURVE ( 'NONE', #1176, #1421, #9813, .T. ) ;
#4290 = DIRECTION ( 'NONE',  ( -0.000000000000000000, -0.000000000000000000, -1.000000000000000000 ) ) ;
#4291 = CARTESIAN_POINT ( 'NONE',  ( -15.29705854078139460, -27.45107625865536605, 4.847467093863555185E-17 ) ) ;
#4292 = CARTESIAN_POINT ( 'NONE',  ( -5.783440176334588401, -75.54545454545275618, -8.231660884606981199 ) ) ;
#4293 = CARTESIAN_POINT ( 'NONE',  ( 25.00000000000000355, 120.0000000000000142, 2.499999999999999556 ) ) ;
#4294 = ADVANCED_FACE ( 'NONE', ( #5673 ), #7764, .T. ) ;
#4295 = DIRECTION ( 'NONE',  ( 6.158143864569485777E-17, 2.736152283717910599E-16, -1.000000000000000000 ) ) ;
#4296 = EDGE_CURVE ( 'NONE', #13011, #6322, #645, .T. ) ;
#4297 = AXIS2_PLACEMENT_3D ( 'NONE', #7006, #11562, #10162 ) ;
#4298 = DIRECTION ( 'NONE',  ( 1.000000000000000000, -1.110223024625156935E-15, 0.000000000000000000 ) ) ;
#4299 = CARTESIAN_POINT ( 'NONE',  ( 34.99999999999958789, 1.104930248025249758E-13, -2.499999999999999112 ) ) ;
#4300 = ORIENTED_EDGE ( 'NONE', *, *, #6429, .F. ) ;
#4301 = DIRECTION ( 'NONE',  ( -2.797435172181481150E-17, 1.000000000000000000, -1.765856845898762549E-18 ) ) ;
#4302 = ORIENTED_EDGE ( 'NONE', *, *, #2844, .F. ) ;
#4303 = DIRECTION ( 'NONE',  ( -2.797435172181481150E-17, 1.000000000000000000, -1.765856845898762549E-18 ) ) ;
#4304 = VERTEX_POINT ( 'NONE', #8821 ) ;
#4305 = CARTESIAN_POINT ( 'NONE',  ( 25.00000000000000355, 120.0000000000000284, -0.5000000000000000000 ) ) ;
#4306 = CARTESIAN_POINT ( 'NONE',  ( 0.000000000000000000, 71.01020514433645303, 2.500000000000000000 ) ) ;
#4307 = CARTESIAN_POINT ( 'NONE',  ( 15.29705854078139637, 0.8232575913729167638, 3.746698755667523989E-15 ) ) ;
#4308 = ADVANCED_FACE ( 'NONE', ( #9955 ), #3772, .T. ) ;
#4309 = CARTESIAN_POINT ( 'NONE',  ( -12.05308885558866550, -134.6363636363568901, 5.101645771607369539 ) ) ;
#4310 = CARTESIAN_POINT ( 'NONE',  ( -8.385254915620295790, 24.75422479069652582, -2.113967306380547611E-15 ) ) ;
#4311 = CARTESIAN_POINT ( 'NONE',  ( 10.69381717166375800, -21.56444287793185666, 0.000000000000000000 ) ) ;
#4312 = EDGE_CURVE ( 'NONE', #12643, #13879, #10846, .T. ) ;
#4313 = DIRECTION ( 'NONE',  ( -0.000000000000000000, -0.000000000000000000, -1.000000000000000000 ) ) ;
#4314 = AXIS2_PLACEMENT_3D ( 'NONE', #4324, #8744, #6569 ) ;
#4315 = DIRECTION ( 'NONE',  ( -6.158143864569485777E-17, -2.736152283717910599E-16, 1.000000000000000000 ) ) ;
#4316 = EDGE_LOOP ( 'NONE', ( #3726, #8280, #12512, #8695 ) ) ;
#4317 = AXIS2_PLACEMENT_3D ( 'NONE', #4140, #6387, #1132 ) ;
#4318 = CARTESIAN_POINT ( 'NONE',  ( 0.000000000000000000, 0.000000000000000000, 0.000000000000000000 ) ) ;
#4319 = ORIENTED_EDGE ( 'NONE', *, *, #8468, .T. ) ;
#4320 = CARTESIAN_POINT ( 'NONE',  ( 15.29705854078139105, 46.06057977201469100, 1.790347283588440782E-15 ) ) ;
#4321 = DIRECTION ( 'NONE',  ( -0.5999999999999989786, -0.8000000000000008216, 0.000000000000000000 ) ) ;
#4322 = DIRECTION ( 'NONE',  ( -2.797435172181481150E-17, 1.000000000000000000, -1.765856845898762549E-18 ) ) ;
#4323 = CARTESIAN_POINT ( 'NONE',  ( -19.75162188639114902, 26.77857048203551926, 3.206191164072789590 ) ) ;
#4324 = CARTESIAN_POINT ( 'NONE',  ( -2.200973885217364349E-15, 78.67828027274755698, -1.389345798431728350E-16 ) ) ;
#4325 = LINE ( 'NONE', #8606, #11617 ) ;
#4326 = EDGE_LOOP ( 'NONE', ( #5462, #135, #6632, #3827 ) ) ;
#4327 = ORIENTED_EDGE ( 'NONE', *, *, #9869, .F. ) ;
#4328 = ORIENTED_EDGE ( 'NONE', *, *, #458, .T. ) ;
#4329 = DIRECTION ( 'NONE',  ( -1.000000000000000000, 0.000000000000000000, 0.000000000000000000 ) ) ;
#4330 = CIRCLE ( 'NONE', #9943, 24.99999999999998934 ) ;
#4331 = PLANE ( 'NONE',  #5327 ) ;
#4332 = CARTESIAN_POINT ( 'NONE',  ( -5.938565187887739683, -74.76276780260269561, -8.199189674694745023 ) ) ;
#4333 = CARTESIAN_POINT ( 'NONE',  ( -42.16244658108818300, 105.4500712252157655, 2.500000000000000000 ) ) ;
#4334 = FACE_OUTER_BOUND ( 'NONE', #13293, .T. ) ;
#4335 = CARTESIAN_POINT ( 'NONE',  ( -2.227027882156173089, -83.13467912880821586, 9.407963499362976378 ) ) ;
#4336 = CARTESIAN_POINT ( 'NONE',  ( 23.18128365339294916, -22.59575057217061556, -6.505213034913026604E-15 ) ) ;
#4337 = ORIENTED_EDGE ( 'NONE', *, *, #4385, .T. ) ;
#4338 = CIRCLE ( 'NONE', #6162, 9.000000000009000800 ) ;
#4339 = ORIENTED_EDGE ( 'NONE', *, *, #9198, .T. ) ;
#4340 = ORIENTED_EDGE ( 'NONE', *, *, #8325, .F. ) ;
#4341 = AXIS2_PLACEMENT_3D ( 'NONE', #2853, #7127, #13625 ) ;
#4342 = ADVANCED_FACE ( 'NONE', ( #6449 ), #7632, .T. ) ;
#4343 = TOROIDAL_SURFACE ( 'NONE', #12464, 16.99999999999998934, 2.000000000000000000 ) ;
#4344 = DIRECTION ( 'NONE',  ( 0.5952233065713573579, -0.8035603370713738647, 0.000000000000000000 ) ) ;
#4345 = ORIENTED_EDGE ( 'NONE', *, *, #5693, .T. ) ;
#4346 = DIRECTION ( 'NONE',  ( 0.9960067511297464593, -0.08927794634716622324, 6.802837160686558945E-17 ) ) ;
#4347 = FILL_AREA_STYLE_COLOUR ( '', #6392 ) ;
#4348 = CARTESIAN_POINT ( 'NONE',  ( 43.29712336220986657, 19.44704974301885159, -2.499999999999993783 ) ) ;
#4349 = CARTESIAN_POINT ( 'NONE',  ( 15.29705854078139105, 8.361467971976955127, 1.858555455282030396E-15 ) ) ;
#4350 = LINE ( 'NONE', #1153, #12365 ) ;
#4351 = DIRECTION ( 'NONE',  ( -0.000000000000000000, -0.000000000000000000, -1.000000000000000000 ) ) ;
#4352 = VECTOR ( 'NONE', #6760, 1000.000000000000000 ) ;
#4353 = CARTESIAN_POINT ( 'NONE',  ( 0.5850150888149016071, -160.9696969693212623, -1.917718896954408336 ) ) ;
#4354 = CARTESIAN_POINT ( 'NONE',  ( -4.840675591955100110, -75.54545454545453254, -8.982239580829959991 ) ) ;
#4355 = LINE ( 'NONE', #5543, #11669 ) ;
#4356 = VECTOR ( 'NONE', #7172, 1000.000000000000000 ) ;
#4357 = CARTESIAN_POINT ( 'NONE',  ( -35.20000000000000995, 106.3999999999999915, 0.5000000000000000000 ) ) ;
#4358 = VERTEX_POINT ( 'NONE', #11777 ) ;
#4359 = EDGE_CURVE ( 'NONE', #3176, #5520, #3307, .T. ) ;
#4360 = CARTESIAN_POINT ( 'NONE',  ( 12.99553232110414491, 1.649976794542512559, 0.000000000000000000 ) ) ;
#4361 = DIRECTION ( 'NONE',  ( 0.000000000000000000, 0.000000000000000000, -1.000000000000000000 ) ) ;
#4362 = ORIENTED_EDGE ( 'NONE', *, *, #6470, .T. ) ;
#4363 = ADVANCED_FACE ( 'NONE', ( #6580 ), #4331, .T. ) ;
#4364 = EDGE_CURVE ( 'NONE', #6810, #8545, #12743, .T. ) ;
#4365 = CYLINDRICAL_SURFACE ( 'NONE', #8179, 15.29705854078139105 ) ;
#4366 = AXIS2_PLACEMENT_3D ( 'NONE', #9492, #11658, #8497 ) ;
#4367 = DIRECTION ( 'NONE',  ( 1.000000000000000000, 0.000000000000000000, 0.000000000000000000 ) ) ;
#4368 = EDGE_CURVE ( 'NONE', #1714, #4148, #12050, .T. ) ;
#4369 = ORIENTED_EDGE ( 'NONE', *, *, #4899, .T. ) ;
#4370 = DIRECTION ( 'NONE',  ( -2.797435172181481150E-17, 1.000000000000000000, -1.765856845898762549E-18 ) ) ;
#4371 = AXIS2_PLACEMENT_3D ( 'NONE', #8289, #7234, #11584 ) ;
#4372 = EDGE_CURVE ( 'NONE', #10190, #9777, #5385, .T. ) ;
#4373 = DIRECTION ( 'NONE',  ( -1.000000000000000000, 0.000000000000000000, 0.000000000000000000 ) ) ;
#4374 = CARTESIAN_POINT ( 'NONE',  ( 15.29705854078139282, 55.48535772202409788, -30.59411708156277854 ) ) ;
#4375 = CARTESIAN_POINT ( 'NONE',  ( 19.50211115783503857, -14.38212227840833179, -2.500000000000004441 ) ) ;
#4376 = DIRECTION ( 'NONE',  ( -2.797435172181481150E-17, 1.000000000000000000, -1.765856845898762549E-18 ) ) ;
#4377 = CYLINDRICAL_SURFACE ( 'NONE', #10445, 2.500000000000002220 ) ;
#4378 = CIRCLE ( 'NONE', #10436, 27.49999999999999289 ) ;
#4379 = CYLINDRICAL_SURFACE ( 'NONE', #4086, 8.385254915620295790 ) ;
#4380 = DIRECTION ( 'NONE',  ( -0.000000000000000000, 0.000000000000000000, -1.000000000000000000 ) ) ;
#4381 = AXIS2_PLACEMENT_3D ( 'NONE', #826, #10154, #6081 ) ;
#4382 = ORIENTED_EDGE ( 'NONE', *, *, #7402, .T. ) ;
#4383 = ADVANCED_FACE ( 'NONE', ( #77, #8614 ), #3286, .F. ) ;
#4384 = ORIENTED_EDGE ( 'NONE', *, *, #8558, .T. ) ;
#4385 = EDGE_CURVE ( 'NONE', #9931, #3127, #10915, .T. ) ;
#4386 = SHAPE_REPRESENTATION_RELATIONSHIP ( 'NONE' , 'NONE' ,  #12318, #3546 ) ;
#4387 = EDGE_LOOP ( 'NONE', ( #459, #9617, #3225, #6736 ) ) ;
#4388 = CARTESIAN_POINT ( 'NONE',  ( -32.50000000000000000, 110.0000000000000142, 2.500000000000000000 ) ) ;
#4389 = CARTESIAN_POINT ( 'NONE',  ( 25.00000000000001776, -99.24349759607916610, 1.707585965103451509 ) ) ;
#4390 = CARTESIAN_POINT ( 'NONE',  ( 39.06230589874905235, 109.5835921350012683, -2.499999999999999556 ) ) ;
#4391 = VECTOR ( 'NONE', #13493, 1000.000000000000000 ) ;
#4392 = DIRECTION ( 'NONE',  ( -0.000000000000000000, -0.000000000000000000, -1.000000000000000000 ) ) ;
#4393 = VERTEX_POINT ( 'NONE', #9811 ) ;
#4394 = ORIENTED_EDGE ( 'NONE', *, *, #5316, .F. ) ;
#4395 = ORIENTED_EDGE ( 'NONE', *, *, #5133, .F. ) ;
#4396 = ADVANCED_FACE ( 'NONE', ( #8684 ), #13127, .F. ) ;
#4397 = EDGE_LOOP ( 'NONE', ( #11029, #9398, #8543, #9771 ) ) ;
#4398 = LINE ( 'NONE', #7627, #13710 ) ;
#4399 = ORIENTED_EDGE ( 'NONE', *, *, #4817, .F. ) ;
#4400 = DIRECTION ( 'NONE',  ( 0.9960067511297464593, -0.08927794634716622324, 3.401418580343279473E-17 ) ) ;
#4401 = DIRECTION ( 'NONE',  ( 0.6000000000000001998, 0.7999999999999999334, 0.000000000000000000 ) ) ;
#4402 = CARTESIAN_POINT ( 'NONE',  ( -34.46489414126432393, 107.6161901685304514, -1.920132901535060777 ) ) ;
#4403 = DIRECTION ( 'NONE',  ( -2.797435172181481150E-17, 1.000000000000000000, -1.765856845898762549E-18 ) ) ;
#4404 = FACE_OUTER_BOUND ( 'NONE', #8429, .T. ) ;
#4405 = CARTESIAN_POINT ( 'NONE',  ( 8.385254915620294014, 24.75422479069652582, 9.855024866598292994E-16 ) ) ;
#4406 = EDGE_LOOP ( 'NONE', ( #1490, #8222, #10555, #8448 ) ) ;
#4407 = B_SPLINE_CURVE_WITH_KNOTS ( 'NONE', 3,
 ( #12183, #6704, #6853, #7678 ),
 .UNSPECIFIED., .F., .F.,
 ( 4, 4 ),
 ( 0.000000000000000000, 1.000000000000000000 ),
 .UNSPECIFIED. ) ;
#4408 = ORIENTED_EDGE ( 'NONE', *, *, #269, .T. ) ;
#4409 = ORIENTED_EDGE ( 'NONE', *, *, #6195, .F. ) ;
#4410 = CARTESIAN_POINT ( 'NONE',  ( -39.06230589874905235, 109.5835921350012683, 2.499999999999999556 ) ) ;
#4411 = ORIENTED_EDGE ( 'NONE', *, *, #10582, .T. ) ;
#4412 = CARTESIAN_POINT ( 'NONE',  ( -15.29705854078139460, -1.063309978032445979, 30.59411708156277854 ) ) ;
#4413 = DIRECTION ( 'NONE',  ( 1.000000000000000000, 0.000000000000000000, 0.000000000000000000 ) ) ;
#4414 = DIRECTION ( 'NONE',  ( -1.000000000000000000, 0.000000000000000000, 0.000000000000000000 ) ) ;
#4415 = CARTESIAN_POINT ( 'NONE',  ( 38.16244658108818300, 102.4500712252157655, -2.500000000000000444 ) ) ;
#4416 = DIRECTION ( 'NONE',  ( 0.4206864060305147146, -0.9072061219927525233, -2.409338161076489703E-16 ) ) ;
#4417 = CARTESIAN_POINT ( 'NONE',  ( -24.99999999999998934, -100.0000000000000000, -7.500000000000000000 ) ) ;
#4418 = CARTESIAN_POINT ( 'NONE',  ( -3.188279143310615904, -76.81818181818212565, -9.710576830322478870 ) ) ;
#4419 = EDGE_CURVE ( 'NONE', #4551, #5287, #13665, .T. ) ;
#4420 = CYLINDRICAL_SURFACE ( 'NONE', #3835, 25.00000000000000355 ) ;
#4421 = DIRECTION ( 'NONE',  ( -0.8000000000000008216, 0.5999999999999988676, 0.000000000000000000 ) ) ;
#4422 = AXIS2_PLACEMENT_3D ( 'NONE', #3925, #12489, #5179 ) ;
#4423 = EDGE_LOOP ( 'NONE', ( #6880, #601, #9700, #3451 ) ) ;
#4424 = FACE_OUTER_BOUND ( 'NONE', #3284, .T. ) ;
#4425 = CARTESIAN_POINT ( 'NONE',  ( 12.99579180576517068, 73.50828762700210461, -25.99158361153033070 ) ) ;
#4426 = ORIENTED_EDGE ( 'NONE', *, *, #10142, .T. ) ;
#4427 = CARTESIAN_POINT ( 'NONE',  ( -52.50000000000000000, 120.0000000000000142, -2.499999999999998668 ) ) ;
#4428 = DIRECTION ( 'NONE',  ( -0.000000000000000000, -0.000000000000000000, -1.000000000000000000 ) ) ;
#4429 = PLANE ( 'NONE',  #12561 ) ;
#4430 = ORIENTED_EDGE ( 'NONE', *, *, #480, .F. ) ;
#4431 = DIRECTION ( 'NONE',  ( -0.000000000000000000, -0.000000000000000000, -1.000000000000000000 ) ) ;
#4432 = VERTEX_POINT ( 'NONE', #13063 ) ;
#4433 = CARTESIAN_POINT ( 'NONE',  ( 35.00000000000000000, 4.286263797015736496E-15, -7.500000000000000000 ) ) ;
#4434 = AXIS2_PLACEMENT_3D ( 'NONE', #9037, #10015, #4682 ) ;
#4435 = CARTESIAN_POINT ( 'NONE',  ( -15.29705854078139460, 55.48535772202409078, -3.843012250319258015E-15 ) ) ;
#4436 = CARTESIAN_POINT ( 'NONE',  ( 34.99999999999958789, 1.104930248025249758E-13, -2.499999999999999112 ) ) ;
#4437 = EDGE_CURVE ( 'NONE', #3113, #6530, #7696, .T. ) ;
#4438 = DIRECTION ( 'NONE',  ( -0.000000000000000000, -0.000000000000000000, -1.000000000000000000 ) ) ;
#4439 = DIRECTION ( 'NONE',  ( -0.6000000000000001998, 0.7999999999999999334, 0.000000000000000000 ) ) ;
#4440 = EDGE_CURVE ( 'NONE', #6322, #13011, #8461, .T. ) ;
#4441 = CARTESIAN_POINT ( 'NONE',  ( -37.50000000000000711, -4.286263797015736496E-15, -7.500000000000000000 ) ) ;
#4442 = CARTESIAN_POINT ( 'NONE',  ( 60.49844721164429728, -0.2814068163155470925, 2.500000000000001332 ) ) ;
#4443 = PLANE ( 'NONE',  #6472 ) ;
#4444 = EDGE_CURVE ( 'NONE', #8621, #5403, #10762, .T. ) ;
#4445 = DIRECTION ( 'NONE',  ( 0.000000000000000000, 0.000000000000000000, 1.000000000000000000 ) ) ;
#4446 = AXIS2_PLACEMENT_3D ( 'NONE', #9899, #3432, #11990 ) ;
#4447 = ORIENTED_EDGE ( 'NONE', *, *, #6628, .T. ) ;
#4448 = FACE_OUTER_BOUND ( 'NONE', #1707, .T. ) ;
#4449 =( NAMED_UNIT ( * ) PLANE_ANGLE_UNIT ( ) SI_UNIT ( $, .RADIAN. ) );
#4450 = EDGE_LOOP ( 'NONE', ( #6346, #8394, #10400, #11834 ) ) ;
#4451 = CARTESIAN_POINT ( 'NONE',  ( 8.385254915620294014, 31.55439052270045508, 9.688596779957294507E-16 ) ) ;
#4452 = ADVANCED_FACE ( 'NONE', ( #6930 ), #1610, .T. ) ;
#4453 = CIRCLE ( 'NONE', #9626, 8.385254915620292238 ) ;
#4454 = DIRECTION ( 'NONE',  ( 1.000000000000000000, 0.000000000000000000, 0.000000000000000000 ) ) ;
#4455 = DIRECTION ( 'NONE',  ( -0.000000000000000000, -0.000000000000000000, -1.000000000000000000 ) ) ;
#4456 = CIRCLE ( 'NONE', #7378, 9.000000000009002576 ) ;
#4457 = DIRECTION ( 'NONE',  ( -2.797435172181481150E-17, 1.000000000000000000, -1.765856845898762549E-18 ) ) ;
#4458 = ADVANCED_FACE ( 'NONE', ( #10306 ), #2414, .T. ) ;
#4459 = VERTEX_POINT ( 'NONE', #579 ) ;
#4460 = EDGE_CURVE ( 'NONE', #5520, #3176, #6018, .T. ) ;
#4461 = VERTEX_POINT ( 'NONE', #1746 ) ;
#4462 = AXIS2_PLACEMENT_3D ( 'NONE', #9784, #13177, #5711 ) ;
#4463 = VECTOR ( 'NONE', #12503, 1000.000000000000114 ) ;
#4464 = AXIS2_PLACEMENT_3D ( 'NONE', #9369, #9440, #952 ) ;
#4465 = AXIS2_PLACEMENT_3D ( 'NONE', #320, #3382, #9991 ) ;
#4466 = VERTEX_POINT ( 'NONE', #7005 ) ;
#4467 = VERTEX_POINT ( 'NONE', #709 ) ;
#4468 = DIRECTION ( 'NONE',  ( -1.000000000000000000, 0.000000000000000000, 0.000000000000000000 ) ) ;
#4469 = EDGE_LOOP ( 'NONE', ( #1325, #9795, #13468, #9680 ) ) ;
#4470 = CARTESIAN_POINT ( 'NONE',  ( -15.29705854078139637, 74.33491362204294717, -2.135879010051317068E-15 ) ) ;
#4471 = ADVANCED_FACE ( 'NONE', ( #10236 ), #2803, .F. ) ;
#4472 = DIRECTION ( 'NONE',  ( -1.000000000000000000, 0.000000000000000000, 0.000000000000000000 ) ) ;
#4473 = EDGE_CURVE ( 'NONE', #4673, #7723, #8977, .T. ) ;
#4474 = CARTESIAN_POINT ( 'NONE',  ( -7.476762168534553332, -73.27151470233611974, -6.844715463267832867 ) ) ;
#4475 = CARTESIAN_POINT ( 'NONE',  ( -2.517691654963332357E-15, 90.00000000000000000, -1.589271161308885878E-16 ) ) ;
#4476 = CARTESIAN_POINT ( 'NONE',  ( -8.385254915620294014, 90.00000000000000000, -1.589271161308885878E-16 ) ) ;
#4477 = CIRCLE ( 'NONE', #1807, 5.000000000000000000 ) ;
#4478 = CARTESIAN_POINT ( 'NONE',  ( -15.29705854078140170, -29.33764382806072746, -3.749737291961210528E-15 ) ) ;
#4479 = CARTESIAN_POINT ( 'NONE',  ( 12.99579180576516890, 26.38439787695498495, 0.000000000000000000 ) ) ;
#4480 = VERTEX_POINT ( 'NONE', #640 ) ;
#4481 = ADVANCED_FACE ( 'NONE', ( #5819 ), #4972, .F. ) ;
#4482 = AXIS2_PLACEMENT_3D ( 'NONE', #1600, #2723, #5884 ) ;
#4483 = CIRCLE ( 'NONE', #12105, 9.000000000008999024 ) ;
#4484 = EDGE_LOOP ( 'NONE', ( #13038, #1541, #520, #3862 ) ) ;
#4485 = EDGE_LOOP ( 'NONE', ( #9194, #3013, #7660, #12086 ) ) ;
#4486 = DIRECTION ( 'NONE',  ( -2.797435172181481150E-17, 1.000000000000000000, -1.765856845898762549E-18 ) ) ;
#4487 = AXIS2_PLACEMENT_3D ( 'NONE', #2470, #11017, #1156 ) ;
#4488 = CARTESIAN_POINT ( 'NONE',  ( 25.00000000000000355, 120.0000000000000142, 0.5000000000000000000 ) ) ;
#4489 = ORIENTED_EDGE ( 'NONE', *, *, #6260, .T. ) ;
#4490 = CARTESIAN_POINT ( 'NONE',  ( 1.958204620527036497E-15, -70.00000000000000000, 1.236099792129133461E-16 ) ) ;
#4491 =( NAMED_UNIT ( * ) SI_UNIT ( $, .STERADIAN. ) SOLID_ANGLE_UNIT ( ) );
#4492 = CARTESIAN_POINT ( 'NONE',  ( 12.99579180576516535, 35.80917582696438473, 3.183050967463142196E-15 ) ) ;
#4493 = AXIS2_PLACEMENT_3D ( 'NONE', #4619, #13770, #11620 ) ;
#4494 = CARTESIAN_POINT ( 'NONE',  ( 12.99579180576516535, 7.534841976936129448, 1.578957136884995801E-15 ) ) ;
#4495 = AXIS2_PLACEMENT_3D ( 'NONE', #2397, #11803, #5419 ) ;
#4496 = CYLINDRICAL_SURFACE ( 'NONE', #4211, 9.000000000008999024 ) ;
#4497 = CARTESIAN_POINT ( 'NONE',  ( 1.111302931123402171, -163.8787878463619734, 2.940232648233732426 ) ) ;
#4498 = CARTESIAN_POINT ( 'NONE',  ( -10.14773761995943069, -69.33333333333402493, 0.3621078539017010822 ) ) ;
#4499 = LINE ( 'NONE', #5622, #12354 ) ;
#4500 = DIRECTION ( 'NONE',  ( 0.9960067511297463483, -0.08927794634716619548, 0.000000000000000000 ) ) ;
#4501 = ORIENTED_EDGE ( 'NONE', *, *, #11606, .T. ) ;
#4502 = AXIS2_PLACEMENT_3D ( 'NONE', #1578, #1778, #5010 ) ;
#4503 = ORIENTED_EDGE ( 'NONE', *, *, #2502, .F. ) ;
#4504 = DIRECTION ( 'NONE',  ( -6.158143864569485777E-17, -2.736152283717910599E-16, 1.000000000000000000 ) ) ;
#4505 = DIRECTION ( 'NONE',  ( 0.000000000000000000, 1.000000000000000000, 0.000000000000000000 ) ) ;
#4506 = ORIENTED_EDGE ( 'NONE', *, *, #5568, .F. ) ;
#4507 = CARTESIAN_POINT ( 'NONE',  ( 0.000000000000000000, 40.00000000000000000, 15.70031846811053455 ) ) ;
#4508 = CARTESIAN_POINT ( 'NONE',  ( -15.29705854078140170, 90.00000000000000000, -1.589271161308885878E-16 ) ) ;
#4509 = CARTESIAN_POINT ( 'NONE',  ( 10.69381717166375090, 25.55944687211528787, 21.38763434332751245 ) ) ;
#4510 = DIRECTION ( 'NONE',  ( 1.000000000000000000, 0.000000000000000000, 0.000000000000000000 ) ) ;
#4511 = DIRECTION ( 'NONE',  ( -2.797435172181481150E-17, 1.000000000000000000, -1.765856845898762549E-18 ) ) ;
#4512 = FACE_OUTER_BOUND ( 'NONE', #2066, .T. ) ;
#4513 = CARTESIAN_POINT ( 'NONE',  ( 10.69381717166375800, -30.98922082794128485, 21.38763434332752666 ) ) ;
#4514 = CARTESIAN_POINT ( 'NONE',  ( -8.385254915620297567, 90.00000000000000000, -1.589271161308885878E-16 ) ) ;
#4515 = FACE_OUTER_BOUND ( 'NONE', #7454, .T. ) ;
#4516 = ORIENTED_EDGE ( 'NONE', *, *, #8243, .T. ) ;
#4517 = CARTESIAN_POINT ( 'NONE',  ( -0.6173387890061912131, -40.00941361824966691, 4.961742921553712549 ) ) ;
#4518 = VERTEX_POINT ( 'NONE', #3848 ) ;
#4519 = EDGE_LOOP ( 'NONE', ( #13835, #11111, #12104, #11102 ) ) ;
#4520 = DIRECTION ( 'NONE',  ( -6.158143864569485777E-17, -2.736152283717910599E-16, 1.000000000000000000 ) ) ;
#4521 = CONTEXT_DEPENDENT_SHAPE_REPRESENTATION ( #12303, #5519 ) ;
#4522 = VERTEX_POINT ( 'NONE', #2596 ) ;
#4523 = CARTESIAN_POINT ( 'NONE',  ( -6.999999999999999112, -35.00000000000000000, -7.500000000000000000 ) ) ;
#4524 = CIRCLE ( 'NONE', #7013, 18.74900000001875000 ) ;
#4525 = CARTESIAN_POINT ( 'NONE',  ( 25.00000000000002487, -99.29838587104471515, 2.138129719433864206 ) ) ;
#4526 = VECTOR ( 'NONE', #334, 1000.000000000000000 ) ;
#4527 = DIRECTION ( 'NONE',  ( -0.000000000000000000, -0.000000000000000000, 1.000000000000000000 ) ) ;
#4528 = FACE_OUTER_BOUND ( 'NONE', #12363, .T. ) ;
#4529 = VERTEX_POINT ( 'NONE', #5742 ) ;
#4530 = ORIENTED_EDGE ( 'NONE', *, *, #6935, .F. ) ;
#4531 = ADVANCED_FACE ( 'NONE', ( #9117 ), #11377, .T. ) ;
#4532 = AXIS2_PLACEMENT_3D ( 'NONE', #2042, #7432, #8172 ) ;
#4533 = CARTESIAN_POINT ( 'NONE',  ( 12.99553232110414136, 29.92431064457076673, 0.000000000000000000 ) ) ;
#4534 = CIRCLE ( 'NONE', #7457, 9.000000000008999024 ) ;
#4535 = EDGE_CURVE ( 'NONE', #4795, #4098, #2520, .T. ) ;
#4536 = ORIENTED_EDGE ( 'NONE', *, *, #9518, .F. ) ;
#4537 = CARTESIAN_POINT ( 'NONE',  ( -25.00000000000000000, -35.00000000000000000, 7.500000000000000000 ) ) ;
#4538 = ORIENTED_EDGE ( 'NONE', *, *, #12547, .F. ) ;
#4539 = EDGE_CURVE ( 'NONE', #149, #11311, #11071, .T. ) ;
#4540 = CARTESIAN_POINT ( 'NONE',  ( 10.69381717166374735, 72.68333662216240043, 21.38763434332750890 ) ) ;
#4541 = ADVANCED_FACE ( 'NONE', ( #13711 ), #12832, .T. ) ;
#4542 = DIRECTION ( 'NONE',  ( -1.000000000000000000, 0.000000000000000000, 0.000000000000000000 ) ) ;
#4543 = AXIS2_PLACEMENT_3D ( 'NONE', #6408, #4295, #4500 ) ;
#4544 = SURFACE_SIDE_STYLE ('',( #5386 ) ) ;
#4545 = DIRECTION ( 'NONE',  ( -2.797435172181481150E-17, 1.000000000000000000, -1.765856845898762549E-18 ) ) ;
#4546 = CARTESIAN_POINT ( 'NONE',  ( 4.330127018922190096, 91.82970358694004176, -2.500000000000000444 ) ) ;
#4547 = CARTESIAN_POINT ( 'NONE',  ( -8.540654091808187687, -91.31629189966393767, 1.858473920087736930 ) ) ;
#4548 = DIRECTION ( 'NONE',  ( -2.797435172181481150E-17, 1.000000000000000000, -1.765856845898762549E-18 ) ) ;
#4549 = ORIENTED_EDGE ( 'NONE', *, *, #6765, .T. ) ;
#4550 = ORIENTED_EDGE ( 'NONE', *, *, #7059, .T. ) ;
#4551 = VERTEX_POINT ( 'NONE', #5177 ) ;
#4552 = CIRCLE ( 'NONE', #6590, 77.99999999999997158 ) ;
#4553 = ORIENTED_EDGE ( 'NONE', *, *, #7477, .F. ) ;
#4554 = CARTESIAN_POINT ( 'NONE',  ( 34.99999999999958789, 1.091249486606660213E-13, 2.500000000000000000 ) ) ;
#4555 = CARTESIAN_POINT ( 'NONE',  ( 8.385254915620292238, 90.00000000000000000, 8.679704431140114636E-16 ) ) ;
#4556 = ORIENTED_EDGE ( 'NONE', *, *, #7807, .F. ) ;
#4557 = CARTESIAN_POINT ( 'NONE',  ( 8.385254915620288685, -3.520109059331755219, 16.77050983124058448 ) ) ;
#4558 =( NAMED_UNIT ( * ) SI_UNIT ( $, .STERADIAN. ) SOLID_ANGLE_UNIT ( ) );
#4559 = CARTESIAN_POINT ( 'NONE',  ( -10.69381717166375800, 34.98422482212468054, 21.38763434332750535 ) ) ;
#4560 = EDGE_CURVE ( 'NONE', #5087, #3748, #11616, .T. ) ;
#4561 = CARTESIAN_POINT ( 'NONE',  ( 8.385254915620292238, 90.00000000000000000, 8.679704431140114636E-16 ) ) ;
#4562 = CARTESIAN_POINT ( 'NONE',  ( 38.89115197531749857, 101.6687180808697377, 2.499999999999999556 ) ) ;
#4563 = CARTESIAN_POINT ( 'NONE',  ( 35.00000000000009237, 91.25000000000046896, 7.500000000000000000 ) ) ;
#4564 = CARTESIAN_POINT ( 'NONE',  ( -8.385254915620297567, 90.00000000000000000, -1.589271161308885878E-16 ) ) ;
#4565 = CARTESIAN_POINT ( 'NONE',  ( 8.385254915620288685, 53.02855864072483882, 9.355740606675293587E-16 ) ) ;
#4566 = CARTESIAN_POINT ( 'NONE',  ( -12.99553232110414847, -17.19957910547634228, 25.99106464220827917 ) ) ;
#4567 = FACE_BOUND ( 'NONE', #6391, .T. ) ;
#4568 = CIRCLE ( 'NONE', #117, 2.000000000000003997 ) ;
#4569 = ORIENTED_EDGE ( 'NONE', *, *, #2863, .T. ) ;
#4570 = ORIENTED_EDGE ( 'NONE', *, *, #4437, .T. ) ;
#4571 = DIRECTION ( 'NONE',  ( 0.1928999275155749149, 0.9812184353977894125, 2.775705599192072226E-16 ) ) ;
#4572 = DIRECTION ( 'NONE',  ( 0.000000000000000000, 0.000000000000000000, 1.000000000000000000 ) ) ;
#4573 = CARTESIAN_POINT ( 'NONE',  ( -10.00000000000000533, 92.00000000000000000, 2.500000000000000000 ) ) ;
#4574 = DIRECTION ( 'NONE',  ( -2.797435172181481150E-17, 1.000000000000000000, -1.765856845898762549E-18 ) ) ;
#4575 = VERTEX_POINT ( 'NONE', #3985 ) ;
#4577 = ORIENTED_EDGE ( 'NONE', *, *, #8238, .T. ) ;
#4576 = AXIS2_PLACEMENT_3D ( 'NONE', #6416, #7460, #885 ) ;
#4578 = DIRECTION ( 'NONE',  ( -0.000000000000000000, -0.000000000000000000, -1.000000000000000000 ) ) ;
#4579 = ORIENTED_EDGE ( 'NONE', *, *, #1463, .F. ) ;
#4580 = DIRECTION ( 'NONE',  ( 0.000000000000000000, 0.000000000000000000, 1.000000000000000000 ) ) ;
#4581 = ADVANCED_FACE ( 'NONE', ( #13839 ), #11561, .T. ) ;
#4582 = CARTESIAN_POINT ( 'NONE',  ( 15.29705854078139105, 27.21102387199583816, 3.746698755667522411E-15 ) ) ;
#4583 = CARTESIAN_POINT ( 'NONE',  ( 35.45454545454547457, 140.4866414850956744, -2.500000000000000000 ) ) ;
#4584 = VECTOR ( 'NONE', #4578, 1000.000000000000000 ) ;
#4585 = CARTESIAN_POINT ( 'NONE',  ( -10.00000000000000711, 139.9999999999999716, -2.500000000000000000 ) ) ;
#4586 = CARTESIAN_POINT ( 'NONE',  ( -38.99475364604207073, 101.5790910151996655, -2.500000000000037748 ) ) ;
#4587 = APPLICATION_CONTEXT ( 'automotive_design' ) ;
#4588 = SURFACE_STYLE_FILL_AREA ( #12758 ) ;
#4589 = CARTESIAN_POINT ( 'NONE',  ( 38.99475364604206362, 101.5790910151996655, 2.500000000000036859 ) ) ;
#4590 = DIRECTION ( 'NONE',  ( -1.000000000000000000, 0.000000000000000000, 0.000000000000000000 ) ) ;
#4591 = CARTESIAN_POINT ( 'NONE',  ( 10.69346802281034847, -6.949821576306441706, 0.000000000000000000 ) ) ;
#4592 = CIRCLE ( 'NONE', #2353, 5.999999999999998224 ) ;
#4593 = ORIENTED_EDGE ( 'NONE', *, *, #6132, .T. ) ;
#4594 = CYLINDRICAL_SURFACE ( 'NONE', #2704, 50.00000000000001421 ) ;
#4595 = ORIENTED_EDGE ( 'NONE', *, *, #5545, .T. ) ;
#4596 = CARTESIAN_POINT ( 'NONE',  ( -0.1852016367018560761, -70.00000000000000000, 1.488522876466114253 ) ) ;
#4597 = AXIS2_PLACEMENT_3D ( 'NONE', #9485, #2966, #6055 ) ;
#4598 = ORIENTED_EDGE ( 'NONE', *, *, #13517, .F. ) ;
#4599 = CARTESIAN_POINT ( 'NONE',  ( 10.11144057928414242, -69.99977036137985920, -0.2534939170199681513 ) ) ;
#4600 = ITEM_DEFINED_TRANSFORMATION ( 'NONE', 'NONE', #8635,  #8193 ) ;
#4601 = EDGE_LOOP ( 'NONE', ( #11008, #7257, #9917, #2629 ) ) ;
#4602 = AXIS2_PLACEMENT_3D ( 'NONE', #3810, #4935, #8163 ) ;
#4603 = DIRECTION ( 'NONE',  ( -6.158143864569485777E-17, -2.736152283717910599E-16, 1.000000000000000000 ) ) ;
#4604 = CARTESIAN_POINT ( 'NONE',  ( -38.99425905299099071, 101.5795188936649254, 2.500000000000002665 ) ) ;
#4605 = AXIS2_PLACEMENT_3D ( 'NONE', #4756, #12112, #10897 ) ;
#4606 = VECTOR ( 'NONE', #13610, 1000.000000000000000 ) ;
#4607 = FACE_OUTER_BOUND ( 'NONE', #3517, .T. ) ;
#4608 = EDGE_CURVE ( 'NONE', #9044, #5648, #6240, .T. ) ;
#4609 = UNCERTAINTY_MEASURE_WITH_UNIT (LENGTH_MEASURE( 1.000000000000000082E-05 ), #4684, 'distance_accuracy_value', 'NONE');
#4610 = CARTESIAN_POINT ( 'NONE',  ( 9.346811155104262525, -72.85217758658251341, 3.836677952648664292 ) ) ;
#4611 = VERTEX_POINT ( 'NONE', #9324 ) ;
#4612 = EDGE_LOOP ( 'NONE', ( #8102, #1205, #6834, #12067 ) ) ;
#4613 = CIRCLE ( 'NONE', #13394, 2.000000000000003997 ) ;
#4614 = CARTESIAN_POINT ( 'NONE',  ( -8.385254915620290461, -24.99427717735608567, -16.77050983124058803 ) ) ;
#4615 = ORIENTED_EDGE ( 'NONE', *, *, #6005, .T. ) ;
#4616 = ORIENTED_EDGE ( 'NONE', *, *, #10569, .T. ) ;
#4617 = DIRECTION ( 'NONE',  ( 0.000000000000000000, 1.000000000000000000, 0.000000000000000000 ) ) ;
#4618 = ORIENTED_EDGE ( 'NONE', *, *, #301, .F. ) ;
#4619 = CARTESIAN_POINT ( 'NONE',  ( 19.50211115783503857, -14.38212227840833179, 2.499999999999995115 ) ) ;
#4620 = VECTOR ( 'NONE', #3273, 1000.000000000000000 ) ;
#4621 = CARTESIAN_POINT ( 'NONE',  ( 5.570495138619319060E-16, -19.91286587805129926, 3.516327053222078456E-17 ) ) ;
#4622 = CARTESIAN_POINT ( 'NONE',  ( 19.87806660956081828, 26.74843260078022311, 2.549167750534976573 ) ) ;
#4623 = CARTESIAN_POINT ( 'NONE',  ( -34.46489652880495669, 107.6161854625081844, 1.920135329999819174 ) ) ;
#4624 = CARTESIAN_POINT ( 'NONE',  ( 3.521437233922025456, 90.23421079890158580, -3.553194557407191034 ) ) ;
#4625 = EDGE_CURVE ( 'NONE', #13124, #6696, #841, .T. ) ;
#4626 = ADVANCED_FACE ( 'NONE', ( #5107 ), #2866, .T. ) ;
#4627 = ORIENTED_EDGE ( 'NONE', *, *, #11484, .F. ) ;
#4628 = ORIENTED_EDGE ( 'NONE', *, *, #7977, .T. ) ;
#4629 = EDGE_CURVE ( 'NONE', #576, #8296, #7416, .T. ) ;
#4630 = ADVANCED_FACE ( 'NONE', ( #4119 ), #374, .T. ) ;
#4631 = ORIENTED_EDGE ( 'NONE', *, *, #13240, .T. ) ;
#4632 = DIRECTION ( 'NONE',  ( -1.000000000000000000, -2.797435172181480534E-17, -0.000000000000000000 ) ) ;
#4633 = VERTEX_POINT ( 'NONE', #9728 ) ;
#4634 = CARTESIAN_POINT ( 'NONE',  ( 6.629834776934352192, -74.11811802551933681, 7.660853572563749658 ) ) ;
#4635 = CARTESIAN_POINT ( 'NONE',  ( 22.00000000000002132, -97.00000000000000000, -7.500000000000000000 ) ) ;
#4636 = CARTESIAN_POINT ( 'NONE',  ( 10.69346802281034670, 59.02362407375952102, -21.38693604562068629 ) ) ;
#4637 = CARTESIAN_POINT ( 'NONE',  ( 34.99999999999958789, 1.091249486606660213E-13, 2.500000000000000000 ) ) ;
#4638 = CARTESIAN_POINT ( 'NONE',  ( 37.50000000000002132, 144.4948974278317735, 2.499999999999999556 ) ) ;
#4639 = CARTESIAN_POINT ( 'NONE',  ( -9.561354441693807661E-16, 34.17900274070598243, -6.035522597566817733E-17 ) ) ;
#4640 = CARTESIAN_POINT ( 'NONE',  ( 9.849578953078907517, -91.60173160171747497, -1.758148290379567769 ) ) ;
#4641 = CARTESIAN_POINT ( 'NONE',  ( 34.99999999999958789, 1.063887963769481123E-13, 12.50000000000000000 ) ) ;
#4642 = VECTOR ( 'NONE', #4202, 999.9999999999998863 ) ;
#4643 = DIRECTION ( 'NONE',  ( 1.000000000000000000, 0.000000000000000000, 0.000000000000000000 ) ) ;
#4644 = DIRECTION ( 'NONE',  ( 1.000000000000000000, 0.000000000000000000, 0.000000000000000000 ) ) ;
#4645 = ORIENTED_EDGE ( 'NONE', *, *, #6212, .T. ) ;
#4646 = ORIENTED_EDGE ( 'NONE', *, *, #10643, .T. ) ;
#4647 = DIRECTION ( 'NONE',  ( 2.797435172181480534E-17, -1.000000000000000000, 1.765856845898762164E-18 ) ) ;
#4648 = ORIENTED_EDGE ( 'NONE', *, *, #8248, .T. ) ;
#4649 = EDGE_CURVE ( 'NONE', #6457, #2481, #919, .T. ) ;
#4650 = EDGE_CURVE ( 'NONE', #5851, #13160, #12505, .T. ) ;
#4651 = DIRECTION ( 'NONE',  ( -0.000000000000000000, -0.000000000000000000, -1.000000000000000000 ) ) ;
#4652 = CYLINDRICAL_SURFACE ( 'NONE', #6487, 24.99999999999998934 ) ;
#4653 = CARTESIAN_POINT ( 'NONE',  ( 50.48962708925064646, 14.39101985375337556, 2.500000000000004885 ) ) ;
#4654 = CARTESIAN_POINT ( 'NONE',  ( 23.18128365339294916, -22.59575057217061556, 2.499999999999992895 ) ) ;
#4655 = ORIENTED_EDGE ( 'NONE', *, *, #6137, .F. ) ;
#4656 = ORIENTED_EDGE ( 'NONE', *, *, #10866, .F. ) ;
#4657 = DIRECTION ( 'NONE',  ( 0.000000000000000000, 0.000000000000000000, 1.000000000000000000 ) ) ;
#4658 = VERTEX_POINT ( 'NONE', #2288 ) ;
#4659 = DIRECTION ( 'NONE',  ( 1.000000000000000000, 3.558407130208836623E-15, 0.000000000000000000 ) ) ;
#4660 = CARTESIAN_POINT ( 'NONE',  ( -25.00000000000000355, 120.0000000000000142, 0.5000000000000000000 ) ) ;
#4661 = CARTESIAN_POINT ( 'NONE',  ( 10.69381717166375267, 72.68333662216238622, 0.000000000000000000 ) ) ;
#4662 = CARTESIAN_POINT ( 'NONE',  ( 15.29705854078138927, 36.63580182200523438, 1.806990092252540434E-15 ) ) ;
#4663 = DIRECTION ( 'NONE',  ( 1.000000000000000000, 0.000000000000000000, 0.000000000000000000 ) ) ;
#4664 = ADVANCED_FACE ( 'NONE', ( #140 ), #13194, .T. ) ;
#4665 = DIRECTION ( 'NONE',  ( -5.337610695313252124E-17, 1.000000000000000000, 0.000000000000000000 ) ) ;
#4666 = AXIS2_PLACEMENT_3D ( 'NONE', #4268, #8284, #4072 ) ;
#4667 = DIRECTION ( 'NONE',  ( -1.000000000000000000, 0.000000000000000000, 0.000000000000000000 ) ) ;
#4668 = CARTESIAN_POINT ( 'NONE',  ( 10.69346802281035202, -6.949821576306441706, -21.38693604562069339 ) ) ;
#4669 = ADVANCED_FACE ( 'NONE', ( #2427 ), #12970, .T. ) ;
#4670 = CARTESIAN_POINT ( 'NONE',  ( 4.330127018922190985, 92.00000000000000000, 2.500000000000000000 ) ) ;
#4671 = VERTEX_POINT ( 'NONE', #7071 ) ;
#4672 = AXIS2_PLACEMENT_3D ( 'NONE', #11967, #6642, #13047 ) ;
#4673 = VERTEX_POINT ( 'NONE', #10698 ) ;
#4674 = AXIS2_PLACEMENT_3D ( 'NONE', #7023, #3797, #1697 ) ;
#4675 = FACE_OUTER_BOUND ( 'NONE', #1039, .T. ) ;
#4676 = APPLICATION_PROTOCOL_DEFINITION ( 'draft international standard', 'automotive_design', 1998, #5047 ) ;
#4677 = ORIENTED_EDGE ( 'NONE', *, *, #2234, .F. ) ;
#4678 = CARTESIAN_POINT ( 'NONE',  ( -49.99999999999999289, 120.0000000000000284, -0.5000000000000000000 ) ) ;
#4679 = CARTESIAN_POINT ( 'NONE',  ( -39.75092559767095679, 101.0685047868946072, 2.236846530894073926 ) ) ;
#4680 = DIRECTION ( 'NONE',  ( 1.000000000000000000, 0.000000000000000000, 0.000000000000000000 ) ) ;
#4681 = AXIS2_PLACEMENT_3D ( 'NONE', #13560, #10364, #3064 ) ;
#4682 = DIRECTION ( 'NONE',  ( -1.000000000000000000, 0.000000000000000000, 0.000000000000000000 ) ) ;
#4683 = AXIS2_PLACEMENT_3D ( 'NONE', #672, #13323, #9225 ) ;
#4684 =( LENGTH_UNIT ( ) NAMED_UNIT ( * ) SI_UNIT ( .MILLI., .METRE. ) );
#4685 = ORIENTED_EDGE ( 'NONE', *, *, #8930, .T. ) ;
#4686 = EDGE_LOOP ( 'NONE', ( #5289, #2437 ) ) ;
#4687 = ORIENTED_EDGE ( 'NONE', *, *, #2997, .T. ) ;
#4688 = LINE ( 'NONE', #9045, #8098 ) ;
#4689 = AXIS2_PLACEMENT_3D ( 'NONE', #4801, #8938, #3513 ) ;
#4690 = DIRECTION ( 'NONE',  ( -1.000000000000000000, 0.000000000000000000, 0.000000000000000000 ) ) ;
#4691 = DIRECTION ( 'NONE',  ( 0.000000000000000000, 1.000000000000000000, 0.000000000000000000 ) ) ;
#4692 = DIRECTION ( 'NONE',  ( 0.000000000000000000, 0.000000000000000000, 1.000000000000000000 ) ) ;
#4693 = CARTESIAN_POINT ( 'NONE',  ( -0.2881385893809246812, -81.23289783331699709, -9.920954048540957970 ) ) ;
#4694 = CARTESIAN_POINT ( 'NONE',  ( 8.385254915620292238, 59.82872437272870769, 2.053795118489800004E-15 ) ) ;
#4695 = ORIENTED_EDGE ( 'NONE', *, *, #8468, .F. ) ;
#4696 = AXIS2_PLACEMENT_3D ( 'NONE', #2117, #3960, #8502 ) ;
#4697 = ORIENTED_EDGE ( 'NONE', *, *, #10470, .T. ) ;
#4698 = CIRCLE ( 'NONE', #4929, 9.000000000008999024 ) ;
#4699 = VECTOR ( 'NONE', #6735, 1000.000000000000000 ) ;
#4700 = EDGE_CURVE ( 'NONE', #849, #575, #2154, .T. ) ;
#4701 = CARTESIAN_POINT ( 'NONE',  ( 15.29705854078139637, -27.45107625865536605, 3.746698755667523989E-15 ) ) ;
#4702 = EDGE_CURVE ( 'NONE', #10679, #3210, #3204, .T. ) ;
#4703 = CARTESIAN_POINT ( 'NONE',  ( -22.42156014662057473, -97.00000000000000000, 7.500000000000000000 ) ) ;
#4704 = EDGE_LOOP ( 'NONE', ( #8540, #6910, #4550, #6702, #1812 ) ) ;
#4705 = CARTESIAN_POINT ( 'NONE',  ( 4.330127018922190985, 92.00000000000000000, 2.500000000000000000 ) ) ;
#4706 = FILL_AREA_STYLE_COLOUR ( '', #10205 ) ;
#4707 = CARTESIAN_POINT ( 'NONE',  ( 8.385254915620285132, 34.17900274070598243, 16.77050983124058092 ) ) ;
#4708 = DIRECTION ( 'NONE',  ( 0.000000000000000000, 1.000000000000000000, 0.000000000000000000 ) ) ;
#4709 = CIRCLE ( 'NONE', #11429, 9.000000000009002576 ) ;
#4710 = DIRECTION ( 'NONE',  ( 1.000000000000000000, 0.000000000000000000, 0.000000000000000000 ) ) ;
#4711 = DIRECTION ( 'NONE',  ( 1.387778780781444492E-15, 1.000000000000000000, -1.734723475976805615E-16 ) ) ;
#4712 = PRODUCT_DEFINITION ( 'UNKNOWN', '', #8199, #5888 ) ;
#4713 = CARTESIAN_POINT ( 'NONE',  ( -6.459897978785787309, -117.0909090909085393, -0.7661034210343102835 ) ) ;
#4714 = CIRCLE ( 'NONE', #4251, 82.49999999999998579 ) ;
#4715 = DIRECTION ( 'NONE',  ( 2.797435172181480534E-17, -1.000000000000000000, 1.765856845898762164E-18 ) ) ;
#4716 = AXIS2_PLACEMENT_3D ( 'NONE', #2093, #9794, #13036 ) ;
#4717 = CARTESIAN_POINT ( 'NONE',  ( 8.385254915620292238, 90.00000000000000000, 8.679704431140114636E-16 ) ) ;
#4718 = ORIENTED_EDGE ( 'NONE', *, *, #686, .T. ) ;
#4719 = ORIENTED_EDGE ( 'NONE', *, *, #5840, .F. ) ;
#4720 = VERTEX_POINT ( 'NONE', #6568 ) ;
#4721 = DIRECTION ( 'NONE',  ( -1.000000000000000000, 0.000000000000000000, 0.000000000000000000 ) ) ;
#4722 = VERTEX_POINT ( 'NONE', #1111 ) ;
#4723 = CARTESIAN_POINT ( 'NONE',  ( 1.149505143677158392, -121.5517071194484089, 4.892824251472469577 ) ) ;
#4724 = DIRECTION ( 'NONE',  ( -1.000000000000000000, 0.000000000000000000, 0.000000000000000000 ) ) ;
#4725 = AXIS2_PLACEMENT_3D ( 'NONE', #10208, #11389, #5013 ) ;
#4726 = AXIS2_PLACEMENT_3D ( 'NONE', #4841, #7922, #1392 ) ;
#4727 = EDGE_CURVE ( 'NONE', #13879, #3176, #5372, .T. ) ;
#4728 = VECTOR ( 'NONE', #429, 1000.000000000000000 ) ;
#4729 = CARTESIAN_POINT ( 'NONE',  ( -15.29705854078139460, -18.02629830864596627, 3.183186227453577089E-17 ) ) ;
#4730 = EDGE_CURVE ( 'NONE', #3489, #4551, #11345, .T. ) ;
#4731 = CYLINDRICAL_SURFACE ( 'NONE', #11434, 15.29705854078139460 ) ;
#4732 = ORIENTED_EDGE ( 'NONE', *, *, #10645, .F. ) ;
#4733 = FACE_OUTER_BOUND ( 'NONE', #3034, .T. ) ;
#4734 = VERTEX_POINT ( 'NONE', #10831 ) ;
#4735 = ADVANCED_FACE ( 'NONE', ( #204 ), #5992, .T. ) ;
#4736 = CARTESIAN_POINT ( 'NONE',  ( 35.00000000000000000, 4.286263797015736496E-15, 7.500000000000000000 ) ) ;
#4737 = CARTESIAN_POINT ( 'NONE',  ( -25.00000000000000355, 120.0000000000000284, -0.5000000000000000000 ) ) ;
#4738 = DIRECTION ( 'NONE',  ( -6.158143864569485777E-17, -2.736152283717910599E-16, 1.000000000000000000 ) ) ;
#4739 = EDGE_CURVE ( 'NONE', #13646, #8612, #8741, .T. ) ;
#4740 = DIRECTION ( 'NONE',  ( 0.000000000000000000, 0.000000000000000000, 1.000000000000000000 ) ) ;
#4741 = EDGE_CURVE ( 'NONE', #3627, #3001, #10923, .T. ) ;
#4742 = CARTESIAN_POINT ( 'NONE',  ( 0.000000000000000000, -20.00000000000000355, 0.000000000000000000 ) ) ;
#4743 = CARTESIAN_POINT ( 'NONE',  ( -18.78199004159287711, 27.01526789321293620, -6.903011289631056258 ) ) ;
#4744 = CARTESIAN_POINT ( 'NONE',  ( 7.000000000000007994, -35.00000000000000000, 7.500000000000000000 ) ) ;
#4745 = CIRCLE ( 'NONE', #13040, 18.74900000001875000 ) ;
#4746 = DIRECTION ( 'NONE',  ( -1.000000000000000000, 0.000000000000000000, 0.000000000000000000 ) ) ;
#4747 = B_SPLINE_CURVE_WITH_KNOTS ( 'NONE', 3,
 ( #657, #3657, #2822, #1629 ),
 .UNSPECIFIED., .F., .F.,
 ( 4, 4 ),
 ( 0.000000000000000000, 1.000000000000000000 ),
 .UNSPECIFIED. ) ;
#4748 = CARTESIAN_POINT ( 'NONE',  ( -2.517691654963332357E-15, 90.00000000000000000, -1.589271161308885878E-16 ) ) ;
#4749 = ORIENTED_EDGE ( 'NONE', *, *, #4440, .T. ) ;
#4750 = ORIENTED_EDGE ( 'NONE', *, *, #9597, .F. ) ;
#4751 = CARTESIAN_POINT ( 'NONE',  ( 25.00000000000000355, 120.0000000000000142, 2.500000000000000000 ) ) ;
#4752 = ADVANCED_FACE ( 'NONE', ( #10980 ), #1492, .F. ) ;
#4753 = ORIENTED_EDGE ( 'NONE', *, *, #6685, .T. ) ;
#4754 = DIRECTION ( 'NONE',  ( -1.000000000000000000, 0.000000000000000000, 0.000000000000000000 ) ) ;
#4755 = AXIS2_PLACEMENT_3D ( 'NONE', #1017, #6791, #4766 ) ;
#4756 = CARTESIAN_POINT ( 'NONE',  ( 0.000000000000000000, 0.000000000000000000, 0.000000000000000000 ) ) ;
#4757 = EDGE_LOOP ( 'NONE', ( #1119, #3428, #4878, #4328 ) ) ;
#4758 = CARTESIAN_POINT ( 'NONE',  ( -11.95302590259205111, -161.0909090909570409, -5.173310689868307222 ) ) ;
#4759 = EDGE_CURVE ( 'NONE', #7271, #717, #3739, .T. ) ;
#4760 = CARTESIAN_POINT ( 'NONE',  ( -15.29705854078139282, 8.361467971976955127, 30.59411708156277498 ) ) ;
#4761 = DIRECTION ( 'NONE',  ( 1.000000000000000000, 0.000000000000000000, 0.000000000000000000 ) ) ;
#4762 = CARTESIAN_POINT ( 'NONE',  ( 8.385254915620295790, -34.41905512736551032, 16.77050983124059513 ) ) ;
#4763 = UNCERTAINTY_MEASURE_WITH_UNIT (LENGTH_MEASURE( 1.000000000000000082E-05 ), #7860, 'distance_accuracy_value', 'NONE');
#4764 = FACE_OUTER_BOUND ( 'NONE', #12154, .T. ) ;
#4765 = ORIENTED_EDGE ( 'NONE', *, *, #5567, .T. ) ;
#4766 = DIRECTION ( 'NONE',  ( -1.000000000000000000, 0.000000000000000000, 0.000000000000000000 ) ) ;
#4767 = EDGE_LOOP ( 'NONE', ( #3587, #10789, #8586, #10566 ) ) ;
#4768 = CARTESIAN_POINT ( 'NONE',  ( 34.99999999999958789, 1.104930248025249758E-13, -2.499999999999999112 ) ) ;
#4769 = EDGE_LOOP ( 'NONE', ( #12214, #1769, #4226, #4894 ) ) ;
#4770 = CARTESIAN_POINT ( 'NONE',  ( 10.69346802281034847, -35.22415542633469698, 1.384126719801006158E-15 ) ) ;
#4771 = CARTESIAN_POINT ( 'NONE',  ( -15.29705854078139105, 76.22148119144830503, -2.142541826566686405E-15 ) ) ;
#4772 = CARTESIAN_POINT ( 'NONE',  ( -36.36363636363635976, 142.2680885707561629, 2.500000000000000000 ) ) ;
#4773 = DIRECTION ( 'NONE',  ( 1.000000000000000000, 0.000000000000000000, 0.000000000000000000 ) ) ;
#4774 = CARTESIAN_POINT ( 'NONE',  ( 3.581682357367548697, -100.7588871204822283, 6.662357539611612367 ) ) ;
#4775 =( BOUNDED_SURFACE ( )  B_SPLINE_SURFACE ( 3, 3, ( 
 ( #7674, #11954, #7404, #6495 ),
 ( #5431, #3328, #1240, #6630 ),
 ( #8876, #8955, #2416, #11194 ),
 ( #3682, #7967, #483, #1369 ) ),
 .UNSPECIFIED., .F., .F., .T. ) 
 B_SPLINE_SURFACE_WITH_KNOTS ( ( 4, 4 ),
 ( 4, 4 ),
 ( 0.000000000000000000, 1.000000000000000000 ),
 ( 0.000000000000000000, 1.000000000000000000 ),
 .UNSPECIFIED. ) 
 GEOMETRIC_REPRESENTATION_ITEM ( )  RATIONAL_B_SPLINE_SURFACE ( (
 ( 1.000000000000000000, 0.3333333333333334259, 0.3333333333333334259, 1.000000000000000000),
 ( 1.000000000000000000, 0.3333333333333334259, 0.3333333333333334259, 1.000000000000000000),
 ( 1.000000000000000000, 0.3333333333333334259, 0.3333333333333334259, 1.000000000000000000),
 ( 1.000000000000000000, 0.3333333333333334259, 0.3333333333333334259, 1.000000000000000000) ) ) 
 REPRESENTATION_ITEM ( '' )  SURFACE ( )  );
#4776 = ORIENTED_EDGE ( 'NONE', *, *, #4050, .F. ) ;
#4777 = CIRCLE ( 'NONE', #8797, 4.999999999999998224 ) ;
#4778 = ORIENTED_EDGE ( 'NONE', *, *, #614, .F. ) ;
#4779 = ORIENTED_EDGE ( 'NONE', *, *, #13832, .F. ) ;
#4780 = AXIS2_PLACEMENT_3D ( 'NONE', #8796, #8722, #2206 ) ;
#4781 = ORIENTED_EDGE ( 'NONE', *, *, #4983, .T. ) ;
#4782 = CARTESIAN_POINT ( 'NONE',  ( 0.000000000000000000, -20.00000000000000000, 20.00000000000000000 ) ) ;
#4783 = CARTESIAN_POINT ( 'NONE',  ( 1.010510313258186077, -79.21212121212082025, 9.990963482113931704 ) ) ;
#4784 = EDGE_LOOP ( 'NONE', ( #8057, #4753, #12087, #6836, #3366 ) ) ;
#4785 = CARTESIAN_POINT ( 'NONE',  ( 4.769557440008696858, 90.26587002877201371, 1.504714191168455617 ) ) ;
#4786 = DIRECTION ( 'NONE',  ( 1.000000000000000000, 0.000000000000000000, 0.000000000000000000 ) ) ;
#4787 = CARTESIAN_POINT ( 'NONE',  ( -3.692320488640446374, -128.7272727272685131, 2.755591346289536059 ) ) ;
#4788 = CARTESIAN_POINT ( 'NONE',  ( 0.000000000000000000, -20.00000000000000355, 15.70031846811053455 ) ) ;
#4789 = CARTESIAN_POINT ( 'NONE',  ( 8.385254915620295790, -15.56949922734665570, 1.052073721316228892E-15 ) ) ;
#4790 = CARTESIAN_POINT ( 'NONE',  ( -4.855892414095311693, -117.0909090909095340, -4.610765637404268702 ) ) ;
#4791 = CARTESIAN_POINT ( 'NONE',  ( 41.99999999999999289, 120.0000000000000142, 2.500000000000000000 ) ) ;
#4792 = CARTESIAN_POINT ( 'NONE',  ( 15.70027825049740500, -16.66645554390144568, 0.3441452025673427118 ) ) ;
#4793 = DIRECTION ( 'NONE',  ( 1.000000000000000000, 0.000000000000000000, 0.000000000000000000 ) ) ;
#4794 = ORIENTED_EDGE ( 'NONE', *, *, #6178, .F. ) ;
#4795 = VERTEX_POINT ( 'NONE', #10159 ) ;
#4796 = EDGE_CURVE ( 'NONE', #8273, #6184, #7828, .T. ) ;
#4797 = AXIS2_PLACEMENT_3D ( 'NONE', #8840, #12070, #1411 ) ;
#4798 = CARTESIAN_POINT ( 'NONE',  ( 0.1617766054438460888, -158.9591451343941344, 1.491567609517463255 ) ) ;
#4799 = ORIENTED_EDGE ( 'NONE', *, *, #3722, .T. ) ;
#4800 = CIRCLE ( 'NONE', #5675, 16.99999999999998934 ) ;
#4801 = CARTESIAN_POINT ( 'NONE',  ( -31.00000000000000711, -4.286263797015736496E-15, -8.499999999999998224 ) ) ;
#4802 = CIRCLE ( 'NONE', #6575, 15.29705854078138927 ) ;
#4803 = CARTESIAN_POINT ( 'NONE',  ( 51.25836974494252019, 19.64472991003004054, 2.500000000000006661 ) ) ;
#4804 = FACE_OUTER_BOUND ( 'NONE', #10031, .T. ) ;
#4805 = ORIENTED_EDGE ( 'NONE', *, *, #7623, .F. ) ;
#4806 = CARTESIAN_POINT ( 'NONE',  ( -41.00000000000000000, -4.286263797015736496E-15, -8.499999999999998224 ) ) ;
#4807 = ORIENTED_EDGE ( 'NONE', *, *, #10458, .T. ) ;
#4808 = CARTESIAN_POINT ( 'NONE',  ( -0.7078152277712073115, -145.1309382821781924, 2.289704460722573387 ) ) ;
#4809 = CARTESIAN_POINT ( 'NONE',  ( 4.974937185533097050, 90.00000000000000000, -0.5000000000000000000 ) ) ;
#4810 = DIRECTION ( 'NONE',  ( -0.000000000000000000, -0.000000000000000000, -1.000000000000000000 ) ) ;
#4811 = AXIS2_PLACEMENT_3D ( 'NONE', #7822, #13039, #4262 ) ;
#4812 = FACE_OUTER_BOUND ( 'NONE', #13187, .T. ) ;
#4813 = DIRECTION ( 'NONE',  ( 0.000000000000000000, 0.000000000000000000, 1.000000000000000000 ) ) ;
#4814 = CYLINDRICAL_SURFACE ( 'NONE', #5073, 9.000000000008999024 ) ;
#4815 = EDGE_CURVE ( 'NONE', #2827, #8984, #13633, .T. ) ;
#4816 = EDGE_CURVE ( 'NONE', #3291, #2525, #5806, .T. ) ;
#4817 = EDGE_CURVE ( 'NONE', #11439, #2969, #6873, .T. ) ;
#4818 = VECTOR ( 'NONE', #6949, 1000.000000000000000 ) ;
#4819 = DIRECTION ( 'NONE',  ( -1.000000000000000000, 0.000000000000000000, 0.000000000000000000 ) ) ;
#4820 = CARTESIAN_POINT ( 'NONE',  ( 1.275238607054845374, -147.1038961039289177, -4.986937111405163492 ) ) ;
#4821 = EDGE_CURVE ( 'NONE', #3641, #5368, #13675, .T. ) ;
#4822 = AXIS2_PLACEMENT_3D ( 'NONE', #12018, #9710, #8653 ) ;
#4823 = EDGE_CURVE ( 'NONE', #1226, #768, #835, .T. ) ;
#4824 = CIRCLE ( 'NONE', #7493, 8.385254915620292238 ) ;
#4825 = ORIENTED_EDGE ( 'NONE', *, *, #26, .T. ) ;
#4826 = CARTESIAN_POINT ( 'NONE',  ( 0.5000000000000032196, -40.00941361824966691, -2.499999999999982236 ) ) ;
#4827 = CARTESIAN_POINT ( 'NONE',  ( 15.29705854078138572, 57.37192529142945574, 1.773704474924340342E-15 ) ) ;
#4828 = SHAPE_DEFINITION_REPRESENTATION ( #13178, #5134 ) ;
#4829 = CARTESIAN_POINT ( 'NONE',  ( 15.29705854078139105, 36.63580182200523438, 1.806990092252540434E-15 ) ) ;
#4830 = CARTESIAN_POINT ( 'NONE',  ( 10.69381717166375623, 6.709890972096427042, 2.619229793989003951E-15 ) ) ;
#4831 = CYLINDRICAL_SURFACE ( 'NONE', #13158, 4.999999999999997335 ) ;
#4832 = DIRECTION ( 'NONE',  ( -6.158143864569485777E-17, -2.736152283717910599E-16, 1.000000000000000000 ) ) ;
#4833 = FACE_OUTER_BOUND ( 'NONE', #2920, .T. ) ;
#4834 = PRESENTATION_LAYER_ASSIGNMENT (  '', '', ( #8623 ) ) ;
#4835 = ADVANCED_FACE ( 'NONE', ( #13276 ), #4831, .T. ) ;
#4836 = ORIENTED_EDGE ( 'NONE', *, *, #2166, .F. ) ;
#4837 = ORIENTED_EDGE ( 'NONE', *, *, #1540, .T. ) ;
#4838 = EDGE_CURVE ( 'NONE', #6056, #3127, #9035, .T. ) ;
#4839 = AXIS2_PLACEMENT_3D ( 'NONE', #12430, #7094, #11302 ) ;
#4840 = ORIENTED_EDGE ( 'NONE', *, *, #744, .T. ) ;
#4841 = CARTESIAN_POINT ( 'NONE',  ( 35.00000000000001421, -34.99999999999999289, 4.000000000000000000 ) ) ;
#4842 = CIRCLE ( 'NONE', #8414, 5.000000000000000000 ) ;
#4843 = CARTESIAN_POINT ( 'NONE',  ( 53.02537423504344360, -5.158573900538657497, -2.499999999999999112 ) ) ;
#4844 = CARTESIAN_POINT ( 'NONE',  ( 19.36040733361900124, 26.87219970003946656, 5.058700639371029872 ) ) ;
#4845 = LINE ( 'NONE', #9120, #2603 ) ;
#4846 = CARTESIAN_POINT ( 'NONE',  ( 6.636652343254445086, -87.27833817527823612, -6.409095190688999466 ) ) ;
#4847 = CARTESIAN_POINT ( 'NONE',  ( 10.69346802281035025, 49.59884612375012836, -21.38693604562069339 ) ) ;
#4848 = CIRCLE ( 'NONE', #12689, 2.500000000000002220 ) ;
#4849 = VERTEX_POINT ( 'NONE', #2579 ) ;
#4850 = EDGE_LOOP ( 'NONE', ( #11065, #5434, #4950, #13553 ) ) ;
#4851 = EDGE_CURVE ( 'NONE', #2577, #7989, #13422, .T. ) ;
#4852 = DIRECTION ( 'NONE',  ( -6.158143864569485777E-17, -2.736152283717910599E-16, 1.000000000000000000 ) ) ;
#4853 = LINE ( 'NONE', #13442, #3216 ) ;
#4854 = CARTESIAN_POINT ( 'NONE',  ( 7.783279735887545847, -74.45454545454821016, 6.359494517302611172 ) ) ;
#4855 = VERTEX_POINT ( 'NONE', #6858 ) ;
#4856 = CARTESIAN_POINT ( 'NONE',  ( 1.381416096079823630, -78.35919756719752627, 10.01283213701209540 ) ) ;
#4857 = DIRECTION ( 'NONE',  ( -2.797435172181481150E-17, 1.000000000000000000, -1.765856845898762549E-18 ) ) ;
#4858 = CARTESIAN_POINT ( 'NONE',  ( -7.670607444602973501, -76.12121212000219828, -4.175606131682665811 ) ) ;
#4859 = DIRECTION ( 'NONE',  ( -0.8000000000000000444, 0.5999999999999999778, 0.000000000000000000 ) ) ;
#4860 = CARTESIAN_POINT ( 'NONE',  ( 42.70768697973989703, 17.09141780026012114, -2.499999999999993783 ) ) ;
#4861 = ORIENTED_EDGE ( 'NONE', *, *, #10805, .T. ) ;
#4862 = ORIENTED_EDGE ( 'NONE', *, *, #2049, .F. ) ;
#4863 = AXIS2_PLACEMENT_3D ( 'NONE', #8456, #8389, #12617 ) ;
#4864 = CARTESIAN_POINT ( 'NONE',  ( 22.00000000000002132, -97.00000000000000000, 7.500000000000000000 ) ) ;
#4865 = ORIENTED_EDGE ( 'NONE', *, *, #27, .F. ) ;
#4866 = CARTESIAN_POINT ( 'NONE',  ( -2.357122643816039087, -126.8853818545090348, 3.740305772406630869 ) ) ;
#4867 = FACE_OUTER_BOUND ( 'NONE', #209, .T. ) ;
#4868 = DIRECTION ( 'NONE',  ( 1.000000000000000000, 0.000000000000000000, 0.000000000000000000 ) ) ;
#4869 = ORIENTED_EDGE ( 'NONE', *, *, #8928, .T. ) ;
#4870 = CARTESIAN_POINT ( 'NONE',  ( 22.42156014662059249, -97.00000000000000000, -7.500000000000000000 ) ) ;
#4871 = CARTESIAN_POINT ( 'NONE',  ( -0.2492428495092258167, -158.6992603437087723, -1.476418605036174725 ) ) ;
#4872 = ADVANCED_FACE ( 'NONE', ( #11136 ), #12012, .T. ) ;
#4873 = CARTESIAN_POINT ( 'NONE',  ( -18.54049621773915746, -20.00000000000000000, 7.500000000000000000 ) ) ;
#4874 = FACE_OUTER_BOUND ( 'NONE', #12736, .T. ) ;
#4875 = CARTESIAN_POINT ( 'NONE',  ( 14.99223790936468603, -6.835163196276449860, -2.500000000000002665 ) ) ;
#4876 = DIRECTION ( 'NONE',  ( 1.000000000000000000, 0.000000000000000000, 0.000000000000000000 ) ) ;
#4877 = FACE_OUTER_BOUND ( 'NONE', #2734, .T. ) ;
#4878 = ORIENTED_EDGE ( 'NONE', *, *, #12549, .F. ) ;
#4879 = CARTESIAN_POINT ( 'NONE',  ( 2.179449471770333435, 90.00000000000000000, 4.500000000000000888 ) ) ;
#4880 = ORIENTED_EDGE ( 'NONE', *, *, #12452, .F. ) ;
#4881 = CARTESIAN_POINT ( 'NONE',  ( 4.364119526983701647, -68.90909090873145715, 1.457038019206917223 ) ) ;
#4882 = ORIENTED_EDGE ( 'NONE', *, *, #6789, .F. ) ;
#4883 = VERTEX_POINT ( 'NONE', #4108 ) ;
#4884 = DIRECTION ( 'NONE',  ( -0.7999999999999977129, -0.6000000000000030864, 0.000000000000000000 ) ) ;
#4885 = CARTESIAN_POINT ( 'NONE',  ( -15.47908363509431595, -16.40738050097609602, -2.711248065311635091 ) ) ;
#4886 = ADVANCED_FACE ( 'NONE', ( #7330 ), #10291, .T. ) ;
#4887 = EDGE_CURVE ( 'NONE', #2529, #5403, #8188, .T. ) ;
#4888 = CARTESIAN_POINT ( 'NONE',  ( -3.682460330434897067, -161.0909090908357371, -2.758257593116285822 ) ) ;
#4889 = CARTESIAN_POINT ( 'NONE',  ( 27.38873514654796537, -24.33759740261775661, -4.000000000000000000 ) ) ;
#4890 = EDGE_CURVE ( 'NONE', #7032, #534, #4176, .T. ) ;
#4891 = CARTESIAN_POINT ( 'NONE',  ( -12.99553232110414491, 20.49953269456136695, 25.99106464220827917 ) ) ;
#4892 = UNCERTAINTY_MEASURE_WITH_UNIT (LENGTH_MEASURE( 1.000000000000000082E-05 ), #2535, 'distance_accuracy_value', 'NONE');
#4893 = CARTESIAN_POINT ( 'NONE',  ( 3.989522629621962579, -78.56682793483436456, 9.305603774495006419 ) ) ;
#4894 = ORIENTED_EDGE ( 'NONE', *, *, #4815, .F. ) ;
#4895 = VECTOR ( 'NONE', #12371, 1000.000000000000000 ) ;
#4896 = ORIENTED_EDGE ( 'NONE', *, *, #2226, .T. ) ;
#4897 = AXIS2_PLACEMENT_3D ( 'NONE', #3351, #218, #4472 ) ;
#4898 = CARTESIAN_POINT ( 'NONE',  ( -1.868713978126510744, -80.62942566232119646, 9.873777329404955339 ) ) ;
#4899 = EDGE_CURVE ( 'NONE', #5287, #10825, #1052, .T. ) ;
#4900 = VERTEX_POINT ( 'NONE', #8326 ) ;
#4901 = AXIS2_PLACEMENT_3D ( 'NONE', #9790, #8725, #6564 ) ;
#4902 = CARTESIAN_POINT ( 'NONE',  ( -8.385254915620295790, -6.144721277337255927, 1.085069813372578838E-17 ) ) ;
#4903 = EDGE_CURVE ( 'NONE', #2222, #13867, #13629, .T. ) ;
#4904 = CARTESIAN_POINT ( 'NONE',  ( 18.54049621773915746, 27.07720798312000809, 7.500000000000000000 ) ) ;
#4905 = ADVANCED_FACE ( 'NONE', ( #4964 ), #13825, .T. ) ;
#4906 = CARTESIAN_POINT ( 'NONE',  ( -34.63132358390376453, 107.2645221665701456, 2.217002873864903911 ) ) ;
#4907 = CARTESIAN_POINT ( 'NONE',  ( -5.609076778736961089, -113.1406196337631229, 2.279675803883993268 ) ) ;
#4908 = CIRCLE ( 'NONE', #4683, 2.000000000000000000 ) ;
#4909 = CARTESIAN_POINT ( 'NONE',  ( 10.69381717166375800, 16.13466892210585257, -21.38763434332750535 ) ) ;
#4910 = ORIENTED_EDGE ( 'NONE', *, *, #6885, .T. ) ;
#4911 = VERTEX_POINT ( 'NONE', #6090 ) ;
#4912 = AXIS2_PLACEMENT_3D ( 'NONE', #12791, #13799, #4149 ) ;
#4913 = EDGE_LOOP ( 'NONE', ( #4750, #2, #6715, #13035 ) ) ;
#4914 = CARTESIAN_POINT ( 'NONE',  ( -35.45454545454546036, 140.4866414850956744, -2.500000000000000000 ) ) ;
#4915 = AXIS2_PLACEMENT_3D ( 'NONE', #12449, #3957, #9359 ) ;
#4916 = EDGE_CURVE ( 'NONE', #6758, #6312, #10361, .T. ) ;
#4917 = LINE ( 'NONE', #10246, #8515 ) ;
#4918 = VERTEX_POINT ( 'NONE', #4172 ) ;
#4919 = LINE ( 'NONE', #3727, #10375 ) ;
#4920 = APPLICATION_PROTOCOL_DEFINITION ( 'draft international standard', 'automotive_design', 1998, #8892 ) ;
#4921 = FACE_OUTER_BOUND ( 'NONE', #13635, .T. ) ;
#4922 = CARTESIAN_POINT ( 'NONE',  ( 2.966263562845762980, -142.5800865801409145, 0.5601050917291978681 ) ) ;
#4923 = EDGE_CURVE ( 'NONE', #3901, #8317, #164, .T. ) ;
#4924 = CARTESIAN_POINT ( 'NONE',  ( 25.00000000000001776, -100.0000000000000000, 7.500000000000000000 ) ) ;
#4925 = AXIS2_PLACEMENT_3D ( 'NONE', #11461, #5011, #1921 ) ;
#4926 = LINE ( 'NONE', #9136, #4895 ) ;
#4927 = LINE ( 'NONE', #4860, #1250 ) ;
#4928 = ORIENTED_EDGE ( 'NONE', *, *, #6323, .T. ) ;
#4929 = AXIS2_PLACEMENT_3D ( 'NONE', #1561, #1770, #2692 ) ;
#4930 = EDGE_LOOP ( 'NONE', ( #11350, #11586, #73, #10437 ) ) ;
#4931 = ORIENTED_EDGE ( 'NONE', *, *, #9279, .F. ) ;
#4932 = DIRECTION ( 'NONE',  ( 0.000000000000000000, 0.000000000000000000, 1.000000000000000000 ) ) ;
#4933 = ORIENTED_EDGE ( 'NONE', *, *, #778, .F. ) ;
#4934 = CARTESIAN_POINT ( 'NONE',  ( 6.207397642386911052, -111.4641340365256355, -0.7891162744033484167 ) ) ;
#4935 = DIRECTION ( 'NONE',  ( 0.5952233065713573579, -0.8035603370713738647, 3.056366244416776485E-15 ) ) ;
#4936 = CIRCLE ( 'NONE', #8724, 3.999999999999996447 ) ;
#4937 = CYLINDRICAL_SURFACE ( 'NONE', #248, 79.99999999999997158 ) ;
#4938 = ORIENTED_EDGE ( 'NONE', *, *, #8857, .T. ) ;
#4939 = CARTESIAN_POINT ( 'NONE',  ( 25.00000000000000355, 120.0000000000000142, -0.5000000000000000000 ) ) ;
#4940 = CARTESIAN_POINT ( 'NONE',  ( 0.7922720876982874971, -124.2424753664742667, -4.680861543279757342 ) ) ;
#4941 = AXIS2_PLACEMENT_3D ( 'NONE', #9579, #12825, #831 ) ;
#4942 = AXIS2_PLACEMENT_3D ( 'NONE', #9605, #11905, #8680 ) ;
#4943 = FACE_OUTER_BOUND ( 'NONE', #3454, .T. ) ;
#4944 = FACE_OUTER_BOUND ( 'NONE', #6413, .T. ) ;
#4945 = DIRECTION ( 'NONE',  ( 0.000000000000000000, 0.000000000000000000, -1.000000000000000000 ) ) ;
#4946 = DIRECTION ( 'NONE',  ( 0.9960067511297464593, -0.08927794634716622324, 3.401418580343279473E-17 ) ) ;
#4947 = CARTESIAN_POINT ( 'NONE',  ( -35.06230589874905235, 106.5835921350012825, 7.500000000000000000 ) ) ;
#4948 = CARTESIAN_POINT ( 'NONE',  ( -15.29705854078139637, 64.91013567203349055, -2.102593392723117370E-15 ) ) ;
#4949 = AXIS2_PLACEMENT_3D ( 'NONE', #10473, #13676, #877 ) ;
#4950 = ORIENTED_EDGE ( 'NONE', *, *, #3680, .T. ) ;
#4951 = CIRCLE ( 'NONE', #4716, 9.000000000008999024 ) ;
#4952 = CARTESIAN_POINT ( 'NONE',  ( 10.69346802281034492, 40.17406817374066463, 0.000000000000000000 ) ) ;
#4953 = ORIENTED_EDGE ( 'NONE', *, *, #12001, .F. ) ;
#4954 = CARTESIAN_POINT ( 'NONE',  ( -0.7140975576127730484, -124.8181818181825093, 13.04184819563903197 ) ) ;
#4955 = ORIENTED_EDGE ( 'NONE', *, *, #4419, .T. ) ;
#4956 = EDGE_LOOP ( 'NONE', ( #9738, #1256, #5576, #3362 ) ) ;
#4957 = FACE_OUTER_BOUND ( 'NONE', #1499, .T. ) ;
#4958 = DIRECTION ( 'NONE',  ( -0.000000000000000000, -0.000000000000000000, -1.000000000000000000 ) ) ;
#4959 = AXIS2_PLACEMENT_3D ( 'NONE', #10801, #2390, #10939 ) ;
#4960 = CARTESIAN_POINT ( 'NONE',  ( -2.920448137081767204, -118.2727272727305063, -4.227847206581263784 ) ) ;
#4961 = CIRCLE ( 'NONE', #6730, 2.000000000000000000 ) ;
#4962 = AXIS2_PLACEMENT_3D ( 'NONE', #12376, #9074, #12233 ) ;
#4963 = CARTESIAN_POINT ( 'NONE',  ( 15.29705854078138394, 8.361467971976955127, 30.59411708156277854 ) ) ;
#4964 = FACE_OUTER_BOUND ( 'NONE', #3348, .T. ) ;
#4965 = DIRECTION ( 'NONE',  ( -0.000000000000000000, 1.000000000000000000, -0.000000000000000000 ) ) ;
#4966 = ORIENTED_EDGE ( 'NONE', *, *, #1994, .F. ) ;
#4967 = ADVANCED_FACE ( 'NONE', ( #13558 ), #9783, .T. ) ;
#4968 = ORIENTED_EDGE ( 'NONE', *, *, #3203, .F. ) ;
#4969 = CIRCLE ( 'NONE', #13280, 2.000000000000003997 ) ;
#4970 = EDGE_LOOP ( 'NONE', ( #5649, #8529, #11734, #5482 ) ) ;
#4971 = DIRECTION ( 'NONE',  ( -1.000000000000000000, -2.835060530349834805E-17, 0.000000000000000000 ) ) ;
#4972 = CYLINDRICAL_SURFACE ( 'NONE', #10490, 14.99999999999998934 ) ;
#4973 = CARTESIAN_POINT ( 'NONE',  ( 56.05919550416194141, -1.881564379087038885, 2.500000000000000888 ) ) ;
#4974 = AXIS2_PLACEMENT_3D ( 'NONE', #7827, #4026, #9367 ) ;
#4975 = CARTESIAN_POINT ( 'NONE',  ( 41.99999999999999289, 120.0000000000000284, 0.5000000000000000000 ) ) ;
#4976 = CARTESIAN_POINT ( 'NONE',  ( -4.163221732489563287, -120.7404873314440295, -2.994388017321735429 ) ) ;
#4977 = DIRECTION ( 'NONE',  ( -1.000000000000000000, 0.000000000000000000, 0.000000000000000000 ) ) ;
#4978 = ADVANCED_FACE ( 'NONE', ( #3909 ), #13502, .T. ) ;
#4979 = ORIENTED_EDGE ( 'NONE', *, *, #1217, .T. ) ;
#4980 = EDGE_CURVE ( 'NONE', #8180, #780, #11571, .T. ) ;
#4981 = LINE ( 'NONE', #3929, #8303 ) ;
#4982 = ADVANCED_FACE ( 'NONE', ( #9649 ), #5298, .T. ) ;
#4983 = EDGE_CURVE ( 'NONE', #8546, #1355, #1266, .T. ) ;
#4984 = ORIENTED_EDGE ( 'NONE', *, *, #2327, .F. ) ;
#4985 = CARTESIAN_POINT ( 'NONE',  ( -4.330127018922195425, 92.00000000000000000, -2.500000000000000000 ) ) ;
#4986 = CARTESIAN_POINT ( 'NONE',  ( 9.977514653935656952, -69.33333333333050064, 0.8249805266091517764 ) ) ;
#4987 = ORIENTED_EDGE ( 'NONE', *, *, #4114, .F. ) ;
#4988 = CARTESIAN_POINT ( 'NONE',  ( 15.29705854078138749, 10.24803554138234496, 1.856918518244839783E-15 ) ) ;
#4989 = FACE_OUTER_BOUND ( 'NONE', #9534, .T. ) ;
#4990 = CARTESIAN_POINT ( 'NONE',  ( 0.4173931308547985108, -102.5454545454719266, -7.668730708680674191 ) ) ;
#4991 = CARTESIAN_POINT ( 'NONE',  ( 34.99999999999958789, 1.104930248025249758E-13, -2.499999999999999112 ) ) ;
#4992 = DIRECTION ( 'NONE',  ( 1.000000000000000000, 0.000000000000000000, 0.000000000000000000 ) ) ;
#4993 = DIRECTION ( 'NONE',  ( 0.9960067511297463483, -0.08927794634716620936, 4.626175998653454121E-17 ) ) ;
#4994 = AXIS2_PLACEMENT_3D ( 'NONE', #13114, #1113, #277 ) ;
#4995 = DIRECTION ( 'NONE',  ( 0.000000000000000000, 0.000000000000000000, 1.000000000000000000 ) ) ;
#4996 = AXIS2_PLACEMENT_3D ( 'NONE', #2140, #4313, #8594 ) ;
#4997 = DIRECTION ( 'NONE',  ( 0.9960067511297464593, -0.08927794634716622324, 6.802837160686558945E-17 ) ) ;
#4998 = VERTEX_POINT ( 'NONE', #1296 ) ;
#4999 = ORIENTED_EDGE ( 'NONE', *, *, #11919, .T. ) ;
#5000 = ORIENTED_EDGE ( 'NONE', *, *, #4887, .F. ) ;
#5001 = CARTESIAN_POINT ( 'NONE',  ( 5.055407487860802185, -107.2968172642280109, -4.489258388536537581 ) ) ;
#5002 = AXIS2_PLACEMENT_3D ( 'NONE', #8629, #1408, #3297 ) ;
#5003 = ADVANCED_FACE ( 'NONE', ( #4512 ), #6424, .T. ) ;
#5004 = FACE_OUTER_BOUND ( 'NONE', #13268, .T. ) ;
#5005 = CIRCLE ( 'NONE', #11712, 4.999999999999997335 ) ;
#5006 = DIRECTION ( 'NONE',  ( -2.797435172181481150E-17, 1.000000000000000000, -1.765856845898762549E-18 ) ) ;
#5007 = DIRECTION ( 'NONE',  ( -1.000000000000000000, 0.000000000000000000, 0.000000000000000000 ) ) ;
#5008 = CARTESIAN_POINT ( 'NONE',  ( 1.008311300638476515, -141.1586168970593178, 2.610279145673827461 ) ) ;
#5009 = CARTESIAN_POINT ( 'NONE',  ( 0.6121604144011097981, -166.5454543771828924, 9.081467142972524442 ) ) ;
#5010 = DIRECTION ( 'NONE',  ( -1.000000000000000000, -1.224646799147353207E-16, 0.000000000000000000 ) ) ;
#5011 = DIRECTION ( 'NONE',  ( 0.000000000000000000, 0.000000000000000000, 1.000000000000000000 ) ) ;
#5012 = DIRECTION ( 'NONE',  ( -6.158143864569485777E-17, -2.736152283717910599E-16, 1.000000000000000000 ) ) ;
#5013 = DIRECTION ( 'NONE',  ( 0.000000000000000000, 0.000000000000000000, 1.000000000000000000 ) ) ;
#5014 = CARTESIAN_POINT ( 'NONE',  ( 8.385254915620295790, 31.55439052270045508, 2.053795118489801188E-15 ) ) ;
#5015 = STYLED_ITEM ( 'NONE', ( #9982 ), #12476 ) ;
#5016 = VERTEX_POINT ( 'NONE', #8794 ) ;
#5017 = PLANE ( 'NONE',  #2690 ) ;
#5018 = ORIENTED_EDGE ( 'NONE', *, *, #13162, .T. ) ;
#5019 = CARTESIAN_POINT ( 'NONE',  ( -4.154595973944846143, -169.0000000000000853, 0.9946518452610447758 ) ) ;
#5020 = ADVANCED_FACE ( 'NONE', ( #6491 ), #5741, .T. ) ;
#5021 = ORIENTED_EDGE ( 'NONE', *, *, #5865, .F. ) ;
#5022 = ORIENTED_EDGE ( 'NONE', *, *, #12971, .T. ) ;
#5023 = AXIS2_PLACEMENT_3D ( 'NONE', #1517, #10648, #10896 ) ;
#5024 = CARTESIAN_POINT ( 'NONE',  ( 39.06230589874905235, 109.5835921350012825, -2.499999999999999556 ) ) ;
#5025 = CARTESIAN_POINT ( 'NONE',  ( -15.18222645069203303, -16.04698886238941924, 4.000000000000000000 ) ) ;
#5026 = CARTESIAN_POINT ( 'NONE',  ( 15.65828099947304253, -22.75074427536019783, 1.322318745440853593 ) ) ;
#5027 = LINE ( 'NONE', #3906, #3667 ) ;
#5028 = DIRECTION ( 'NONE',  ( 0.000000000000000000, 0.000000000000000000, 1.000000000000000000 ) ) ;
#5029 = CARTESIAN_POINT ( 'NONE',  ( -25.00000000000000355, 120.0000000000000284, -0.5000000000000000000 ) ) ;
#5030 = CARTESIAN_POINT ( 'NONE',  ( 10.29982004912478821, -6.336490384724132952, -2.500000000000002665 ) ) ;
#5031 = CIRCLE ( 'NONE', #6587, 2.000000000000003109 ) ;
#5032 = DIRECTION ( 'NONE',  ( 1.000000000000000000, -0.000000000000000000, 0.000000000000000000 ) ) ;
#5033 = AXIS2_PLACEMENT_3D ( 'NONE', #7528, #52, #11609 ) ;
#5034 = ORIENTED_EDGE ( 'NONE', *, *, #11404, .F. ) ;
#5035 = VECTOR ( 'NONE', #757, 1000.000000000000000 ) ;
#5036 = ORIENTED_EDGE ( 'NONE', *, *, #1750, .F. ) ;
#5037 = EDGE_LOOP ( 'NONE', ( #11213, #10722, #9721, #3181 ) ) ;
#5038 = CARTESIAN_POINT ( 'NONE',  ( -12.99579180576516535, -20.73949187309215247, -25.99158361153034136 ) ) ;
#5039 = AXIS2_PLACEMENT_3D ( 'NONE', #4736, #3749, #8032 ) ;
#5040 = LINE ( 'NONE', #7863, #766 ) ;
#5041 = ADVANCED_FACE ( 'NONE', ( #8523 ), #10426, .T. ) ;
#5042 = CARTESIAN_POINT ( 'NONE',  ( 26.79177319725820539, -26.24642857144861807, -4.000000000000000000 ) ) ;
#5043 = VECTOR ( 'NONE', #4370, 1000.000000000000000 ) ;
#5044 = CARTESIAN_POINT ( 'NONE',  ( 8.385254915620290461, 62.45333659073423860, 9.189312520034297072E-16 ) ) ;
#5045 = FACE_OUTER_BOUND ( 'NONE', #12481, .T. ) ;
#5046 = CARTESIAN_POINT ( 'NONE',  ( 2.621224576962791986, -142.3792347905090594, 0.5672744485101375300 ) ) ;
#5047 = APPLICATION_CONTEXT ( 'automotive_design' ) ;
#5048 = DIRECTION ( 'NONE',  ( 2.797435172181480534E-17, -1.000000000000000000, 1.765856845898762164E-18 ) ) ;
#5049 = ORIENTED_EDGE ( 'NONE', *, *, #3191, .T. ) ;
#5050 = AXIS2_PLACEMENT_3D ( 'NONE', #5765, #13454, #13304 ) ;
#5051 = CARTESIAN_POINT ( 'NONE',  ( 15.29705854078138927, -8.601520358636511432, 30.59411708156278564 ) ) ;
#5052 = PRESENTATION_LAYER_ASSIGNMENT (  '', '', ( #1461 ) ) ;
#5053 = AXIS2_PLACEMENT_3D ( 'NONE', #1908, #7302, #5197 ) ;
#5054 = VERTEX_POINT ( 'NONE', #8720 ) ;
#5055 = CARTESIAN_POINT ( 'NONE',  ( 52.85884796071297131, 5.708463060827149604, -2.499999999999996447 ) ) ;
#5056 = ORIENTED_EDGE ( 'NONE', *, *, #4289, .T. ) ;
#5057 = CARTESIAN_POINT ( 'NONE',  ( 9.314636722532569024, -70.78787878787778709, 4.145366960882150842 ) ) ;
#5058 = ORIENTED_EDGE ( 'NONE', *, *, #5095, .F. ) ;
#5059 = DIRECTION ( 'NONE',  ( -1.224646799147353207E-16, 1.000000000000000000, -0.000000000000000000 ) ) ;
#5060 = EDGE_CURVE ( 'NONE', #12157, #11361, #13414, .T. ) ;
#5061 = CARTESIAN_POINT ( 'NONE',  ( -7.181435285655783041, -97.41991341991587205, -5.065585088375700096 ) ) ;
#5062 = CARTESIAN_POINT ( 'NONE',  ( 60.47785218637952198, 1.062566689801824893, 2.500000000000001776 ) ) ;
#5063 = AXIS2_PLACEMENT_3D ( 'NONE', #12746, #7401, #13508 ) ;
#5064 = DIRECTION ( 'NONE',  ( -0.9960067511297463483, 0.08927794634716620936, -4.818676322152979407E-17 ) ) ;
#5065 = CARTESIAN_POINT ( 'NONE',  ( -2.179449471770338320, 90.00000000000000000, 4.500000000000000888 ) ) ;
#5066 = CARTESIAN_POINT ( 'NONE',  ( -1.778232137369847088, -131.6676658674560940, 3.416367881604213785 ) ) ;
#5067 = AXIS2_PLACEMENT_3D ( 'NONE', #11688, #10632, #9586 ) ;
#5068 = DIRECTION ( 'NONE',  ( -1.224646799147353207E-16, 1.000000000000000000, -0.000000000000000000 ) ) ;
#5069 = AXIS2_PLACEMENT_3D ( 'NONE', #12540, #7056, #9163 ) ;
#5070 = EDGE_CURVE ( 'NONE', #8647, #6878, #623, .T. ) ;
#5071 = ORIENTED_EDGE ( 'NONE', *, *, #2672, .F. ) ;
#5072 = ORIENTED_EDGE ( 'NONE', *, *, #13852, .F. ) ;
#5073 = AXIS2_PLACEMENT_3D ( 'NONE', #3605, #2636, #412 ) ;
#5074 = DIRECTION ( 'NONE',  ( -6.158143864569485777E-17, -2.736152283717910599E-16, 1.000000000000000000 ) ) ;
#5075 = CARTESIAN_POINT ( 'NONE',  ( 0.4950592182222878224, -80.00113774393089727, 9.987843023254374231 ) ) ;
#5076 = DIRECTION ( 'NONE',  ( -1.000000000000000000, 0.000000000000000000, 0.000000000000000000 ) ) ;
#5077 = CARTESIAN_POINT ( 'NONE',  ( 8.218400508506594093, -92.47990103503111925, 2.510678252300570623 ) ) ;
#5078 = DIRECTION ( 'NONE',  ( -6.158143864569485777E-17, -2.736152283717910599E-16, 1.000000000000000000 ) ) ;
#5079 = ADVANCED_FACE ( 'NONE', ( #2279 ), #10819, .T. ) ;
#5080 = CARTESIAN_POINT ( 'NONE',  ( 0.7584178690488649899, -80.00107432488880477, -10.05132151820344966 ) ) ;
#5081 = DIRECTION ( 'NONE',  ( 0.000000000000000000, 0.000000000000000000, 1.000000000000000000 ) ) ;
#5082 = CARTESIAN_POINT ( 'NONE',  ( -10.69346802281034847, 2.474956373702985157, -2.628033278317404684E-15 ) ) ;
#5083 = DIRECTION ( 'NONE',  ( 0.000000000000000000, 1.000000000000000000, 0.000000000000000000 ) ) ;
#5084 = EDGE_CURVE ( 'NONE', #1705, #9083, #12171, .T. ) ;
#5085 = CARTESIAN_POINT ( 'NONE',  ( 10.69346802281034137, 30.74929022373127196, 21.38693604562069339 ) ) ;
#5086 = ADVANCED_FACE ( 'NONE', ( #9924, #8871 ), #2565, .F. ) ;
#5087 = VERTEX_POINT ( 'NONE', #12247 ) ;
#5088 = FACE_OUTER_BOUND ( 'NONE', #7462, .T. ) ;
#5089 = DIRECTION ( 'NONE',  ( 0.000000000000000000, 0.000000000000000000, 1.000000000000000000 ) ) ;
#5090 = CARTESIAN_POINT ( 'NONE',  ( 82.09155748149851206, -71.43674177705591433, 2.500000000000000000 ) ) ;
#5091 = VERTEX_POINT ( 'NONE', #477 ) ;
#5092 = CARTESIAN_POINT ( 'NONE',  ( -4.804172150869138846, 90.20479154739604155, -1.391179344134541473 ) ) ;
#5093 = CARTESIAN_POINT ( 'NONE',  ( 0.000000000000000000, 71.01020514433645303, 2.500000000000000000 ) ) ;
#5094 = CARTESIAN_POINT ( 'NONE',  ( 7.670607446487990977, -76.12121213288367017, 4.175606128970697384 ) ) ;
#5095 = EDGE_CURVE ( 'NONE', #1278, #5338, #55, .T. ) ;
#5096 = CARTESIAN_POINT ( 'NONE',  ( 57.42269783589186005, -167.3636363757462391, -5.376878111557598316 ) ) ;
#5097 = DIRECTION ( 'NONE',  ( 0.000000000000000000, 0.000000000000000000, 1.000000000000000000 ) ) ;
#5098 = CARTESIAN_POINT ( 'NONE',  ( 34.99999999999958789, 1.063887963769481123E-13, 12.50000000000000000 ) ) ;
#5099 = EDGE_CURVE ( 'NONE', #4069, #3488, #9557, .T. ) ;
#5100 = DIRECTION ( 'NONE',  ( -1.000000000000000000, 0.000000000000000000, 0.000000000000000000 ) ) ;
#5101 = CARTESIAN_POINT ( 'NONE',  ( -4.545390705139096710, 90.76307318580400363, 2.092381513276357463 ) ) ;
#5102 = EDGE_LOOP ( 'NONE', ( #6963, #3129, #756, #2643 ) ) ;
#5103 = CARTESIAN_POINT ( 'NONE',  ( -8.724264547992721219, -88.38328649526096115, 2.552360124988750645 ) ) ;
#5104 = ORIENTED_EDGE ( 'NONE', *, *, #4923, .T. ) ;
#5105 = CARTESIAN_POINT ( 'NONE',  ( 12.99579180576516890, -11.31471392308272605, 1.630544471709826084E-15 ) ) ;
#5106 = CARTESIAN_POINT ( 'NONE',  ( -37.50000000000000711, -4.286263797015736496E-15, 7.500000000000000000 ) ) ;
#5107 = FACE_OUTER_BOUND ( 'NONE', #2816, .T. ) ;
#5108 = CARTESIAN_POINT ( 'NONE',  ( -10.69381717166375090, -2.714886977913000710, -21.38763434332751245 ) ) ;
#5109 = TOROIDAL_SURFACE ( 'NONE', #1527, 16.99999999999998934, 2.000000000000000000 ) ;
#5110 = DIRECTION ( 'NONE',  ( -0.000000000000000000, -0.000000000000000000, -1.000000000000000000 ) ) ;
#5111 = AXIS2_PLACEMENT_3D ( 'NONE', #3556, #5896, #3709 ) ;
#5112 = ORIENTED_EDGE ( 'NONE', *, *, #8243, .F. ) ;
#5113 = FACE_OUTER_BOUND ( 'NONE', #2952, .T. ) ;
#5114 = AXIS2_PLACEMENT_3D ( 'NONE', #335, #7742, #13261 ) ;
#5115 = ORIENTED_EDGE ( 'NONE', *, *, #5924, .T. ) ;
#5116 = EDGE_LOOP ( 'NONE', ( #7504, #12044, #5593, #6502 ) ) ;
#5117 = CARTESIAN_POINT ( 'NONE',  ( 14.13596196814457606, -39.17949320881311337, 1.792870180259218362E-15 ) ) ;
#5118 = ORIENTED_EDGE ( 'NONE', *, *, #13773, .F. ) ;
#5119 = DIRECTION ( 'NONE',  ( 0.000000000000000000, 1.000000000000000000, 1.734723475976805615E-16 ) ) ;
#5120 = CIRCLE ( 'NONE', #11831, 15.29705854078139460 ) ;
#5121 = CARTESIAN_POINT ( 'NONE',  ( 8.385254915620285132, 43.60378069071538221, 16.77050983124058092 ) ) ;
#5122 = DIRECTION ( 'NONE',  ( -6.158143864569485777E-17, -2.736152283717910599E-16, 1.000000000000000000 ) ) ;
#5123 = CARTESIAN_POINT ( 'NONE',  ( 12.99553232110414136, 20.49953269456136695, 0.000000000000000000 ) ) ;
#5124 = CARTESIAN_POINT ( 'NONE',  ( 22.00000000000002132, -100.0000000000000000, 7.500000000000000000 ) ) ;
#5125 = CARTESIAN_POINT ( 'NONE',  ( 1.857895717451711892, -124.7597759017244528, 4.290688988966868678 ) ) ;
#5126 = FACE_OUTER_BOUND ( 'NONE', #5614, .T. ) ;
#5127 = ORIENTED_EDGE ( 'NONE', *, *, #2832, .T. ) ;
#5128 = ORIENTED_EDGE ( 'NONE', *, *, #9776, .T. ) ;
#5129 = CIRCLE ( 'NONE', #886, 8.385254915620295790 ) ;
#5130 = EDGE_LOOP ( 'NONE', ( #1352, #6047, #8763, #10175 ) ) ;
#5131 = FACE_OUTER_BOUND ( 'NONE', #10860, .T. ) ;
#5132 = EDGE_LOOP ( 'NONE', ( #13795, #11373, #1072, #4300 ) ) ;
#5133 = EDGE_CURVE ( 'NONE', #10906, #1805, #2732, .T. ) ;
#5134 = SHAPE_REPRESENTATION ( 'Soft-Touch Grip Cap Sleeve', ( #8193 ), #1690 ) ;
#5135 = CARTESIAN_POINT ( 'NONE',  ( 8.385254915620290461, 40.97916847270985841, 16.77050983124059158 ) ) ;
#5136 = ORIENTED_EDGE ( 'NONE', *, *, #8223, .F. ) ;
#5137 = CARTESIAN_POINT ( 'NONE',  ( 12.99553232110413781, 39.34908859458022334, 1.535118538324121067E-15 ) ) ;
#5138 = CARTESIAN_POINT ( 'NONE',  ( 7.900400410507671722, -86.42170959821115162, -4.992527905362919682 ) ) ;
#5139 = CIRCLE ( 'NONE', #4241, 9.000000000008999024 ) ;
#5140 = CARTESIAN_POINT ( 'NONE',  ( -1.824130267666668859, -166.5454545046794408, 2.249022964271035985 ) ) ;
#5141 = CYLINDRICAL_SURFACE ( 'NONE', #12084, 8.385254915620292238 ) ;
#5142 = DIRECTION ( 'NONE',  ( -0.000000000000000000, -0.000000000000000000, -1.000000000000000000 ) ) ;
#5143 = CIRCLE ( 'NONE', #7819, 14.99999999999998934 ) ;
#5144 = CARTESIAN_POINT ( 'NONE',  ( 32.05482125692310547, -25.32934902781012099, -2.500000000000006217 ) ) ;
#5145 = CARTESIAN_POINT ( 'NONE',  ( -15.29705854078139282, 29.09759144140119957, 30.59411708156277498 ) ) ;
#5146 = CARTESIAN_POINT ( 'NONE',  ( -15.29705854078138749, 38.52236939141059935, -6.802498971006334016E-17 ) ) ;
#5147 = EDGE_CURVE ( 'NONE', #6243, #3832, #11353, .T. ) ;
#5148 = ORIENTED_EDGE ( 'NONE', *, *, #8413, .F. ) ;
#5149 = LINE ( 'NONE', #3243, #5364 ) ;
#5150 = AXIS2_PLACEMENT_3D ( 'NONE', #4003, #11368, #13586 ) ;
#5151 = CARTESIAN_POINT ( 'NONE',  ( -12.87330105402729785, -111.7272727272713553, 6.772701765862009893 ) ) ;
#5152 = ADVANCED_FACE ( 'NONE', ( #7810 ), #550, .T. ) ;
#5153 = ORIENTED_EDGE ( 'NONE', *, *, #2781, .T. ) ;
#5154 = VECTOR ( 'NONE', #8915, 1000.000000000000000 ) ;
#5155 = CARTESIAN_POINT ( 'NONE',  ( -27.38873514654796537, -24.33759740261776017, -4.000000000000000000 ) ) ;
#5156 = ADVANCED_FACE ( 'NONE', ( #2489 ), #3752, .F. ) ;
#5157 = EDGE_LOOP ( 'NONE', ( #1442, #4179, #4245, #11293 ) ) ;
#5158 = CARTESIAN_POINT ( 'NONE',  ( 25.00000000000000355, 120.0000000000000142, 2.500000000000000000 ) ) ;
#5159 = EDGE_CURVE ( 'NONE', #10377, #10478, #4197, .T. ) ;
#5160 = DIRECTION ( 'NONE',  ( 1.000000000000000000, 0.000000000000000000, 0.000000000000000000 ) ) ;
#5161 = CARTESIAN_POINT ( 'NONE',  ( 14.88155114952949276, -22.23162151614121029, 5.171026666816163520 ) ) ;
#5162 = CARTESIAN_POINT ( 'NONE',  ( -17.09331748273503848, -62.63636360940330405, -11.08568378743039595 ) ) ;
#5163 = VECTOR ( 'NONE', #1049, 1000.000000000000000 ) ;
#5164 = DIRECTION ( 'NONE',  ( -5.337610695313252124E-17, 1.000000000000000000, 0.000000000000000000 ) ) ;
#5165 = CIRCLE ( 'NONE', #10093, 5.999999999999998224 ) ;
#5166 = CARTESIAN_POINT ( 'NONE',  ( 25.00000000000000355, 120.0000000000000142, -2.499999999999998668 ) ) ;
#5167 = AXIS2_PLACEMENT_3D ( 'NONE', #7107, #740, #12384 ) ;
#5168 = DIRECTION ( 'NONE',  ( 0.6466635011015220424, 0.7627754036039191554, 8.974258851345311771E-16 ) ) ;
#5169 = EDGE_LOOP ( 'NONE', ( #3760, #1938, #12185, #12270 ) ) ;
#5170 = ADVANCED_FACE ( 'NONE', ( #1436 ), #3070, .F. ) ;
#5171 = CIRCLE ( 'NONE', #13014, 14.99999999999999822 ) ;
#5172 = EDGE_CURVE ( 'NONE', #1257, #3094, #2848, .T. ) ;
#5173 = AXIS2_PLACEMENT_3D ( 'NONE', #282, #506, #6793 ) ;
#5174 = ORIENTED_EDGE ( 'NONE', *, *, #9297, .T. ) ;
#5175 = CARTESIAN_POINT ( 'NONE',  ( -31.00000000000000711, -4.286263797015736496E-15, 8.499999999999998224 ) ) ;
#5176 = CARTESIAN_POINT ( 'NONE',  ( 34.99999999999958789, 1.104930248025249758E-13, -2.499999999999999112 ) ) ;
#5177 = CARTESIAN_POINT ( 'NONE',  ( 48.00000000000000000, 120.0000000000000284, -2.500000000000000000 ) ) ;
#5178 = CARTESIAN_POINT ( 'NONE',  ( 0.000000000000000000, 71.01020514433645303, 0.5000000000000000000 ) ) ;
#5179 = DIRECTION ( 'NONE',  ( 0.000000000000000000, 0.000000000000000000, 1.000000000000000000 ) ) ;
#5180 = TOROIDAL_SURFACE ( 'NONE', #6987, 48.00000000000001421, 2.000000000000000000 ) ;
#5181 = VERTEX_POINT ( 'NONE', #13256 ) ;
#5182 = DIRECTION ( 'NONE',  ( -2.797435172181481150E-17, 1.000000000000000000, -1.765856845898762549E-18 ) ) ;
#5183 = VERTEX_POINT ( 'NONE', #7738 ) ;
#5184 = ORIENTED_EDGE ( 'NONE', *, *, #4903, .T. ) ;
#5185 = DIRECTION ( 'NONE',  ( 0.000000000000000000, 0.000000000000000000, 1.000000000000000000 ) ) ;
#5186 = CARTESIAN_POINT ( 'NONE',  ( -12.99553232110413425, 77.04820039461787928, -25.99106464220827561 ) ) ;
#5187 = ORIENTED_EDGE ( 'NONE', *, *, #4851, .F. ) ;
#5188 = CARTESIAN_POINT ( 'NONE',  ( 31.28009342530033265, 25.22721338310704908, -2.499999999999992450 ) ) ;
#5189 =( BOUNDED_SURFACE ( )  B_SPLINE_SURFACE ( 3, 3, ( 
 ( #13722, #4132, #10585, #2882 ),
 ( #5117, #7155, #1832, #4193 ),
 ( #2957, #8478, #8350, #11573 ),
 ( #6116, #9406, #10389, #9340 ) ),
 .UNSPECIFIED., .F., .F., .T. ) 
 B_SPLINE_SURFACE_WITH_KNOTS ( ( 4, 4 ),
 ( 4, 4 ),
 ( 0.000000000000000000, 1.000000000000000000 ),
 ( 0.000000000000000000, 1.000000000000000000 ),
 .UNSPECIFIED. ) 
 GEOMETRIC_REPRESENTATION_ITEM ( )  RATIONAL_B_SPLINE_SURFACE ( (
 ( 1.000000000000000000, 0.3333333333333334259, 0.3333333333333334259, 1.000000000000000000),
 ( 1.000000000000000000, 0.3333333333333334259, 0.3333333333333334259, 1.000000000000000000),
 ( 1.000000000000000000, 0.3333333333333334259, 0.3333333333333334259, 1.000000000000000000),
 ( 1.000000000000000000, 0.3333333333333334259, 0.3333333333333334259, 1.000000000000000000) ) ) 
 REPRESENTATION_ITEM ( '' )  SURFACE ( )  );
#5190 = CIRCLE ( 'NONE', #8764, 14.99999999999998934 ) ;
#5191 = DIRECTION ( 'NONE',  ( 0.000000000000000000, 0.000000000000000000, 1.000000000000000000 ) ) ;
#5192 = DIRECTION ( 'NONE',  ( 0.9960067511297464593, -0.08927794634716622324, 6.802837160686558945E-17 ) ) ;
#5193 = CARTESIAN_POINT ( 'NONE',  ( -8.355259927329338865, -76.12121211926928765, -3.018973158331568651 ) ) ;
#5194 = CARTESIAN_POINT ( 'NONE',  ( 0.000000000000000000, -100.0000000000000000, 0.000000000000000000 ) ) ;
#5195 = CARTESIAN_POINT ( 'NONE',  ( -8.385254915620292238, 69.25350232273815720, -16.77050983124058803 ) ) ;
#5196 = CARTESIAN_POINT ( 'NONE',  ( 2.559300467072437968, -107.2281355222008159, -6.269538958562518083 ) ) ;
#5197 = DIRECTION ( 'NONE',  ( -0.5999999999999989786, 0.8000000000000008216, 0.000000000000000000 ) ) ;
#5198 = EDGE_LOOP ( 'NONE', ( #11587, #9300, #9779, #11473 ) ) ;
#5199 = ORIENTED_EDGE ( 'NONE', *, *, #3184, .F. ) ;
#5200 = ORIENTED_EDGE ( 'NONE', *, *, #12273, .T. ) ;
#5201 = DIRECTION ( 'NONE',  ( -2.797435172181481150E-17, 1.000000000000000000, -1.765856845898762549E-18 ) ) ;
#5202 = VERTEX_POINT ( 'NONE', #1656 ) ;
#5203 = CARTESIAN_POINT ( 'NONE',  ( 34.99999999999958789, 1.104930248025249758E-13, -2.499999999999999112 ) ) ;
#5204 = VECTOR ( 'NONE', #8792, 1000.000000000000000 ) ;
#5205 = CARTESIAN_POINT ( 'NONE',  ( -5.939735700749026570, -113.5442540614846365, -1.042476841765012985 ) ) ;
#5206 = CARTESIAN_POINT ( 'NONE',  ( 26.69171018101576465, -19.44228176112429551, 2.499999999999994227 ) ) ;
#5207 = CARTESIAN_POINT ( 'NONE',  ( -8.385254915620288685, 62.45333659073424570, -16.77050983124058092 ) ) ;
#5208 = AXIS2_PLACEMENT_3D ( 'NONE', #11887, #13031, #1174 ) ;
#5209 = FACE_OUTER_BOUND ( 'NONE', #9247, .T. ) ;
#5210 = DIRECTION ( 'NONE',  ( -1.000000000000000000, 0.000000000000000000, 0.000000000000000000 ) ) ;
#5211 = EDGE_CURVE ( 'NONE', #10135, #4575, #5531, .T. ) ;
#5212 = DIRECTION ( 'NONE',  ( -0.5999999999999989786, 0.8000000000000008216, 0.000000000000000000 ) ) ;
#5213 = DIRECTION ( 'NONE',  ( 1.000000000000000000, 0.000000000000000000, 0.000000000000000000 ) ) ;
#5214 = DIRECTION ( 'NONE',  ( -6.158143864569485777E-17, -2.736152283717910599E-16, 1.000000000000000000 ) ) ;
#5215 = DIRECTION ( 'NONE',  ( -6.158143864569485777E-17, -2.736152283717910599E-16, 1.000000000000000000 ) ) ;
#5216 = CARTESIAN_POINT ( 'NONE',  ( -2.503528417663017258, -105.1818181818192812, 12.81920766435409931 ) ) ;
#5217 = VERTEX_POINT ( 'NONE', #11580 ) ;
#5218 = CARTESIAN_POINT ( 'NONE',  ( -8.385254915620294014, 90.00000000000000000, -1.589271161308885878E-16 ) ) ;
#5219 = ORIENTED_EDGE ( 'NONE', *, *, #12536, .F. ) ;
#5220 = DIRECTION ( 'NONE',  ( -2.797435172181481150E-17, 1.000000000000000000, -1.765856845898762549E-18 ) ) ;
#5221 = DIRECTION ( 'NONE',  ( -0.000000000000000000, -0.000000000000000000, -1.000000000000000000 ) ) ;
#5222 = DIRECTION ( 'NONE',  ( -1.000000000000000000, 0.000000000000000000, 0.000000000000000000 ) ) ;
#5223 = VECTOR ( 'NONE', #12290, 1000.000000000000114 ) ;
#5224 = CARTESIAN_POINT ( 'NONE',  ( -2.078065351797288685, -164.3636363689741984, 0.8722068071970994207 ) ) ;
#5225 = EDGE_CURVE ( 'NONE', #11226, #12718, #2169, .T. ) ;
#5226 = DIRECTION ( 'NONE',  ( 0.000000000000000000, 0.000000000000000000, 1.000000000000000000 ) ) ;
#5227 = CARTESIAN_POINT ( 'NONE',  ( -15.29705854078139460, 47.94714734142005597, 30.59411708156277498 ) ) ;
#5228 = EDGE_CURVE ( 'NONE', #9113, #2556, #2858, .T. ) ;
#5229 = EDGE_CURVE ( 'NONE', #8317, #5237, #4274, .T. ) ;
#5230 = DIRECTION ( 'NONE',  ( 0.1234677578012386701, 0.000000000000000000, -0.9923485843107424653 ) ) ;
#5231 = DIRECTION ( 'NONE',  ( 0.7627754036039191554, -0.6466635011015219314, 8.673617379884041389E-16 ) ) ;
#5232 = EDGE_CURVE ( 'NONE', #10350, #9880, #11325, .T. ) ;
#5233 = EDGE_CURVE ( 'NONE', #534, #2631, #1513, .T. ) ;
#5234 = ORIENTED_EDGE ( 'NONE', *, *, #12455, .F. ) ;
#5235 = TOROIDAL_SURFACE ( 'NONE', #328, -34.24999999999974420, 66.24999999999978684 ) ;
#5236 = DIRECTION ( 'NONE',  ( 0.000000000000000000, 0.000000000000000000, 1.000000000000000000 ) ) ;
#5237 = VERTEX_POINT ( 'NONE', #2777 ) ;
#5238 = FACE_OUTER_BOUND ( 'NONE', #6965, .T. ) ;
#5239 = LINE ( 'NONE', #12629, #3014 ) ;
#5240 = ADVANCED_FACE ( 'NONE', ( #12390 ), #1720, .T. ) ;
#5241 = CARTESIAN_POINT ( 'NONE',  ( 15.29705854078139282, 29.09759144140119957, -30.59411708156276788 ) ) ;
#5242 = CIRCLE ( 'NONE', #9507, 2.000000000000001776 ) ;
#5243 = CARTESIAN_POINT ( 'NONE',  ( -5.799822669222908011, -77.11029879918604024, -8.314269053643187135 ) ) ;
#5244 = CARTESIAN_POINT ( 'NONE',  ( 2.879696806288778888, -140.3684069432085266, -0.06694681502240752702 ) ) ;
#5245 = DIRECTION ( 'NONE',  ( 0.000000000000000000, 0.000000000000000000, 1.000000000000000000 ) ) ;
#5246 = ORIENTED_EDGE ( 'NONE', *, *, #1914, .T. ) ;
#5247 = EDGE_CURVE ( 'NONE', #11915, #13399, #13333, .T. ) ;
#5248 = ORIENTED_EDGE ( 'NONE', *, *, #12552, .F. ) ;
#5249 = LINE ( 'NONE', #8474, #5371 ) ;
#5250 = AXIS2_PLACEMENT_3D ( 'NONE', #2988, #6419, #6285 ) ;
#5251 = DIRECTION ( 'NONE',  ( -2.797435172181481150E-17, 1.000000000000000000, -1.765856845898762549E-18 ) ) ;
#5252 = ORIENTED_EDGE ( 'NONE', *, *, #13339, .F. ) ;
#5253 = CARTESIAN_POINT ( 'NONE',  ( -10.69346802281034670, 77.87317997377837742, -21.38693604562070050 ) ) ;
#5254 = AXIS2_PLACEMENT_3D ( 'NONE', #13754, #12950, #10682 ) ;
#5255 = ORIENTED_EDGE ( 'NONE', *, *, #11471, .T. ) ;
#5256 = DIRECTION ( 'NONE',  ( -2.797435172181481150E-17, 1.000000000000000000, -1.765856845898762549E-18 ) ) ;
#5257 = DIRECTION ( 'NONE',  ( -0.9960067511297463483, 0.08927794634716618161, -4.818676322152979407E-17 ) ) ;
#5258 = LINE ( 'NONE', #10325, #12782 ) ;
#5259 = CARTESIAN_POINT ( 'NONE',  ( -34.73643445648811934, 107.0738672501280604, -2.329477027598934491 ) ) ;
#5260 = PLANE ( 'NONE',  #8137 ) ;
#5261 = CARTESIAN_POINT ( 'NONE',  ( 4.723947684841503403, -119.5046656414372990, 2.345268719995682538 ) ) ;
#5262 = CARTESIAN_POINT ( 'NONE',  ( 34.66997162884352690, 21.14050806081579736, -2.499999999999992895 ) ) ;
#5263 = CIRCLE ( 'NONE', #7716, 9.000000000008999024 ) ;
#5264 = ORIENTED_EDGE ( 'NONE', *, *, #11606, .F. ) ;
#5265 = EDGE_CURVE ( 'NONE', #7235, #8382, #2538, .T. ) ;
#5266 = ORIENTED_EDGE ( 'NONE', *, *, #7684, .T. ) ;
#5267 = AXIS2_PLACEMENT_3D ( 'NONE', #12659, #941, #10466 ) ;
#5268 = ORIENTED_EDGE ( 'NONE', *, *, #2209, .T. ) ;
#5269 = CARTESIAN_POINT ( 'NONE',  ( 1.204398987562338208, -146.6404311885195568, -1.908543418242987677 ) ) ;
#5270 = CARTESIAN_POINT ( 'NONE',  ( 22.31663499682298735, 16.91633092580596198, -2.499999999999995559 ) ) ;
#5271 = LINE ( 'NONE', #9423, #11188 ) ;
#5272 = ORIENTED_EDGE ( 'NONE', *, *, #7784, .T. ) ;
#5273 = VECTOR ( 'NONE', #1712, 1000.000000000000000 ) ;
#5274 = FACE_OUTER_BOUND ( 'NONE', #5169, .T. ) ;
#5275 = CARTESIAN_POINT ( 'NONE',  ( 7.633069938044322100, -93.52166883861728763, 3.640362836796851465 ) ) ;
#5276 = CARTESIAN_POINT ( 'NONE',  ( 25.00000000000000355, 120.0000000000000142, 0.5000000000000000000 ) ) ;
#5277 = DIRECTION ( 'NONE',  ( 6.158143864569485777E-17, 2.736152283717910599E-16, -1.000000000000000000 ) ) ;
#5278 =( GEOMETRIC_REPRESENTATION_CONTEXT ( 3 ) GLOBAL_UNCERTAINTY_ASSIGNED_CONTEXT ( ( #7685 ) ) GLOBAL_UNIT_ASSIGNED_CONTEXT ( ( #8533, #4449, #3333 ) ) REPRESENTATION_CONTEXT ( 'NONE', 'WORKASPACE' ) );
#5279 = CARTESIAN_POINT ( 'NONE',  ( -15.29705854078139105, 19.67281349139177138, -3.783103832178228351E-15 ) ) ;
#5280 = CIRCLE ( 'NONE', #7486, 22.99999999999999645 ) ;
#5281 = CARTESIAN_POINT ( 'NONE',  ( -9.536547895815854048, -71.90909090909266865, -3.228601540706718787 ) ) ;
#5282 = CARTESIAN_POINT ( 'NONE',  ( 25.00000000000001421, -99.15310334213019416, -0.8520627238942191095 ) ) ;
#5283 = CARTESIAN_POINT ( 'NONE',  ( 12.99579180576516713, -1.889935973073297859, 0.000000000000000000 ) ) ;
#5284 = EDGE_LOOP ( 'NONE', ( #3970, #8862, #9147, #8681 ) ) ;
#5285 = AXIS2_PLACEMENT_3D ( 'NONE', #4333, #12853, #9814 ) ;
#5286 = CARTESIAN_POINT ( 'NONE',  ( 0.000000000000000000, -20.00000000000000000, 0.000000000000000000 ) ) ;
#5287 = VERTEX_POINT ( 'NONE', #9229 ) ;
#5288 = CARTESIAN_POINT ( 'NONE',  ( -12.85629483955644581, -68.90909090901422474, 2.086541329742040318 ) ) ;
#5289 = ORIENTED_EDGE ( 'NONE', *, *, #9614, .F. ) ;
#5290 = CARTESIAN_POINT ( 'NONE',  ( 38.24615002434714484, 18.46584715143433542, -2.499999999999993783 ) ) ;
#5291 = ORIENTED_EDGE ( 'NONE', *, *, #5466, .T. ) ;
#5292 = FACE_OUTER_BOUND ( 'NONE', #1200, .T. ) ;
#5293 = CARTESIAN_POINT ( 'NONE',  ( -2.517691654963332357E-15, 90.00000000000000000, -1.589271161308885878E-16 ) ) ;
#5294 = AXIS2_PLACEMENT_3D ( 'NONE', #630, #1451, #6998 ) ;
#5295 = CARTESIAN_POINT ( 'NONE',  ( 8.943257790336033963, -76.35064935063256542, 10.27353203465967546 ) ) ;
#5296 = CARTESIAN_POINT ( 'NONE',  ( -22.42156014662057473, -97.00000000000000000, -7.500000000000000000 ) ) ;
#5297 = CARTESIAN_POINT ( 'NONE',  ( 10.69346802281034492, 11.89973432371241380, 1.298086082554878758E-15 ) ) ;
#5298 =( BOUNDED_SURFACE ( )  B_SPLINE_SURFACE ( 3, 3, ( 
 ( #2204, #4238, #13028, #126 ),
 ( #5297, #8593, #13890, #9851 ),
 ( #12826, #10623, #7471, #3192 ),
 ( #6560, #3258, #5562, #11813 ) ),
 .UNSPECIFIED., .F., .F., .F. ) 
 B_SPLINE_SURFACE_WITH_KNOTS ( ( 4, 4 ),
 ( 4, 4 ),
 ( 0.000000000000000000, 1.000000000000000000 ),
 ( 0.000000000000000000, 1.000000000000000000 ),
 .UNSPECIFIED. ) 
 GEOMETRIC_REPRESENTATION_ITEM ( )  RATIONAL_B_SPLINE_SURFACE ( (
 ( 1.000000000000000000, 0.3333333333333334259, 0.3333333333333334259, 1.000000000000000000),
 ( 1.000000000000000000, 0.3333333333333334259, 0.3333333333333334259, 1.000000000000000000),
 ( 1.000000000000000000, 0.3333333333333334259, 0.3333333333333334259, 1.000000000000000000),
 ( 1.000000000000000000, 0.3333333333333334259, 0.3333333333333334259, 1.000000000000000000) ) ) 
 REPRESENTATION_ITEM ( '' )  SURFACE ( )  );
#5299 = DIRECTION ( 'NONE',  ( -0.000000000000000000, -0.000000000000000000, 1.000000000000000000 ) ) ;
#5300 = CARTESIAN_POINT ( 'NONE',  ( -8.385254915620292238, 53.02855864072483882, -9.364084330386787485E-17 ) ) ;
#5301 = CARTESIAN_POINT ( 'NONE',  ( 45.47624229149391084, 15.54906262289183871, 2.500000000000004885 ) ) ;
#5302 = ORIENTED_EDGE ( 'NONE', *, *, #6430, .T. ) ;
#5303 = EDGE_CURVE ( 'NONE', #12212, #3703, #5389, .T. ) ;
#5304 = ADVANCED_FACE ( 'NONE', ( #10274 ), #5260, .F. ) ;
#5305 = VERTEX_POINT ( 'NONE', #3892 ) ;
#5306 = EDGE_CURVE ( 'NONE', #7989, #4069, #9702, .T. ) ;
#5307 = DIRECTION ( 'NONE',  ( 0.000000000000000000, 0.000000000000000000, 1.000000000000000000 ) ) ;
#5308 = DIRECTION ( 'NONE',  ( 1.000000000000000000, 0.000000000000000000, 0.000000000000000000 ) ) ;
#5309 = AXIS2_PLACEMENT_3D ( 'NONE', #10207, #615, #676 ) ;
#5310 = CARTESIAN_POINT ( 'NONE',  ( -8.385254915620294014, 53.02855864072483882, 16.77050983124057737 ) ) ;
#5311 = CARTESIAN_POINT ( 'NONE',  ( -5.049283603320642300, -77.73593560939509928, -8.777052014093525756 ) ) ;
#5312 = DIRECTION ( 'NONE',  ( -1.000000000000000000, 0.000000000000000000, 0.000000000000000000 ) ) ;
#5313 = CARTESIAN_POINT ( 'NONE',  ( -29.00000000000000355, -3.551475717527324818E-15, 10.49999999999999822 ) ) ;
#5314 = ORIENTED_EDGE ( 'NONE', *, *, #1669, .F. ) ;
#5315 = ORIENTED_EDGE ( 'NONE', *, *, #7900, .F. ) ;
#5316 = EDGE_CURVE ( 'NONE', #11767, #11197, #3714, .T. ) ;
#5317 = AXIS2_PLACEMENT_3D ( 'NONE', #8338, #12630, #12693 ) ;
#5318 = CARTESIAN_POINT ( 'NONE',  ( -15.29705854078139282, 90.00000000000000000, -1.589271161308885878E-16 ) ) ;
#5319 = ORIENTED_EDGE ( 'NONE', *, *, #17, .F. ) ;
#5320 = CARTESIAN_POINT ( 'NONE',  ( 8.385254915620292238, 90.00000000000000000, 8.679704431140114636E-16 ) ) ;
#5321 = ORIENTED_EDGE ( 'NONE', *, *, #3172, .T. ) ;
#5322 = EDGE_CURVE ( 'NONE', #12944, #9535, #12714, .T. ) ;
#5323 = CARTESIAN_POINT ( 'NONE',  ( -12.99579180576517068, 73.50828762700209040, -1.851135709604445740E-15 ) ) ;
#5324 = ADVANCED_FACE ( 'NONE', ( #1972 ), #1905, .T. ) ;
#5325 = CARTESIAN_POINT ( 'NONE',  ( 10.00000000000000000, 99.99999999999994316, 0.5000000000000000000 ) ) ;
#5326 = CARTESIAN_POINT ( 'NONE',  ( -10.00000000000000000, 98.00000000000000000, 2.500000000000000000 ) ) ;
#5327 = AXIS2_PLACEMENT_3D ( 'NONE', #2165, #10713, #4401 ) ;
#5328 = CARTESIAN_POINT ( 'NONE',  ( -34.63116476221792794, 107.2647840444379312, -2.216888271186469250 ) ) ;
#5329 = CARTESIAN_POINT ( 'NONE',  ( 10.00000000000000000, 90.00000000000000000, 2.500000000000000000 ) ) ;
#5330 = CARTESIAN_POINT ( 'NONE',  ( -2.974680683949035842, -139.3888474069737242, 0.4051703307436435031 ) ) ;
#5331 = CARTESIAN_POINT ( 'NONE',  ( 34.99999999999958789, 1.063887963769481123E-13, 12.50000000000000000 ) ) ;
#5332 = ORIENTED_EDGE ( 'NONE', *, *, #2936, .T. ) ;
#5333 = ORIENTED_EDGE ( 'NONE', *, *, #5133, .T. ) ;
#5334 = ORIENTED_EDGE ( 'NONE', *, *, #8399, .F. ) ;
#5335 = EDGE_CURVE ( 'NONE', #3347, #3846, #8617, .T. ) ;
#5336 = AXIS2_PLACEMENT_3D ( 'NONE', #1761, #10250, #5909 ) ;
#5337 = DIRECTION ( 'NONE',  ( 0.8035603370713739757, 0.5952233065713573579, 0.000000000000000000 ) ) ;
#5338 = VERTEX_POINT ( 'NONE', #1196 ) ;
#5339 = FACE_OUTER_BOUND ( 'NONE', #4265, .T. ) ;
#5340 = CARTESIAN_POINT ( 'NONE',  ( 8.729408204557921991, -88.40583805251594640, -2.523542145620374377 ) ) ;
#5341 = EDGE_CURVE ( 'NONE', #3627, #12589, #12136, .T. ) ;
#5342 = DIRECTION ( 'NONE',  ( -0.000000000000000000, -0.000000000000000000, -1.000000000000000000 ) ) ;
#5343 = CARTESIAN_POINT ( 'NONE',  ( 10.69381717166375623, 63.25855867215300066, -21.38763434332750535 ) ) ;
#5344 = CARTESIAN_POINT ( 'NONE',  ( 35.00000000000000000, 4.286263797015736496E-15, 7.500000000000000000 ) ) ;
#5345 = CARTESIAN_POINT ( 'NONE',  ( -1.010510313258165205, -79.21212121212225554, -9.990963482113517813 ) ) ;
#5346 = FACE_OUTER_BOUND ( 'NONE', #379, .T. ) ;
#5347 = LINE ( 'NONE', #8576, #12410 ) ;
#5348 = CLOSED_SHELL ( 'NONE', ( #7075, #11998, #12703, #8925, #11450, #10014, #13692, #5636, #3628, #12289, #4383, #7452, #10791, #4458 ) ) ;
#5349 = ORIENTED_EDGE ( 'NONE', *, *, #1217, .F. ) ;
#5350 = EDGE_LOOP ( 'NONE', ( #11505, #1771, #11142, #7646 ) ) ;
#5351 = CARTESIAN_POINT ( 'NONE',  ( 12.99579180576516890, -11.31471392308272605, 3.183050967463142591E-15 ) ) ;
#5352 = AXIS2_PLACEMENT_3D ( 'NONE', #10792, #8765, #1203 ) ;
#5353 = ORIENTED_EDGE ( 'NONE', *, *, #9597, .T. ) ;
#5354 = CARTESIAN_POINT ( 'NONE',  ( -37.50000000000002132, 144.4948974278317735, -2.499999999999998668 ) ) ;
#5355 = CYLINDRICAL_SURFACE ( 'NONE', #1010, 8.385254915620294014 ) ;
#5356 = CARTESIAN_POINT ( 'NONE',  ( -1.111721538976399026, -76.35064935050264978, -4.681383094379441445 ) ) ;
#5357 = DIRECTION ( 'NONE',  ( -0.000000000000000000, -0.000000000000000000, -1.000000000000000000 ) ) ;
#5358 = CARTESIAN_POINT ( 'NONE',  ( 8.385254915620295790, 24.75422479069652937, -16.77050983124058448 ) ) ;
#5359 = EDGE_CURVE ( 'NONE', #3971, #8890, #5005, .T. ) ;
#5360 = DIRECTION ( 'NONE',  ( -0.000000000000000000, -0.000000000000000000, -1.000000000000000000 ) ) ;
#5361 = FACE_OUTER_BOUND ( 'NONE', #1353, .T. ) ;
#5362 = AXIS2_PLACEMENT_3D ( 'NONE', #7514, #12000, #10936 ) ;
#5363 = DIRECTION ( 'NONE',  ( 1.000000000000000000, 0.000000000000000000, 0.000000000000000000 ) ) ;
#5364 = VECTOR ( 'NONE', #2191, 1000.000000000000000 ) ;
#5365 = AXIS2_PLACEMENT_3D ( 'NONE', #7424, #3998, #3081 ) ;
#5366 = ORIENTED_EDGE ( 'NONE', *, *, #4823, .T. ) ;
#5367 = AXIS2_PLACEMENT_3D ( 'NONE', #6875, #13363, #3711 ) ;
#5368 = VERTEX_POINT ( 'NONE', #8758 ) ;
#5369 = CARTESIAN_POINT ( 'NONE',  ( 8.385254915620292238, 69.25350232273815720, 2.053795118489800793E-15 ) ) ;
#5370 = VECTOR ( 'NONE', #1032, 1000.000000000000000 ) ;
#5371 = VECTOR ( 'NONE', #2027, 1000.000000000000000 ) ;
#5372 = LINE ( 'NONE', #3472, #4620 ) ;
#5373 = CARTESIAN_POINT ( 'NONE',  ( -10.00000000000000000, 92.00000000000000000, 2.500000000000000000 ) ) ;
#5374 = CARTESIAN_POINT ( 'NONE',  ( 23.10070469010960537, -97.98123128958475547, 7.500000000000000000 ) ) ;
#5375 = EDGE_CURVE ( 'NONE', #8314, #1753, #11077, .T. ) ;
#5376 = FACE_OUTER_BOUND ( 'NONE', #6217, .T. ) ;
#5377 = ORIENTED_EDGE ( 'NONE', *, *, #9258, .F. ) ;
#5378 = CIRCLE ( 'NONE', #9202, 8.385254915620292238 ) ;
#5379 = VERTEX_POINT ( 'NONE', #2523 ) ;
#5380 = CIRCLE ( 'NONE', #4261, 14.99999999999998934 ) ;
#5381 = VERTEX_POINT ( 'NONE', #3422 ) ;
#5382 = DIRECTION ( 'NONE',  ( 0.000000000000000000, 0.000000000000000000, -1.000000000000000000 ) ) ;
#5383 = ORIENTED_EDGE ( 'NONE', *, *, #11920, .F. ) ;
#5384 = DIRECTION ( 'NONE',  ( -0.4545454545454531425, 0.8907235428302472391, 0.000000000000000000 ) ) ;
#5385 = LINE ( 'NONE', #9672, #13202 ) ;
#5386 = SURFACE_STYLE_FILL_AREA ( #5457 ) ;
#5387 = CIRCLE ( 'NONE', #8994, 15.29705854078139282 ) ;
#5388 = CARTESIAN_POINT ( 'NONE',  ( 40.05868326948369429, 100.9130297721161043, -2.014878269406404687 ) ) ;
#5389 = LINE ( 'NONE', #6007, #11041 ) ;
#5390 = EDGE_CURVE ( 'NONE', #3518, #7666, #3288, .T. ) ;
#5391 = B_SPLINE_CURVE_WITH_KNOTS ( 'NONE', 3,
 ( #4183, #5442, #9662, #4323, #8604, #9730, #332, #7811, #3963, #12392, #552, #7181, #4743, #1657 ),
 .UNSPECIFIED., .F., .F.,
 ( 4, 2, 2, 2, 2, 2, 4 ),
 ( 0.000000000000000000, 0.003826572935444120041, 0.005739859403166178327, 0.007653145870888238347, 0.01147971880633235318, 0.01339300527405441234, 0.01530629174177646976 ),
 .UNSPECIFIED. ) ;
#5392 = AXIS2_PLACEMENT_3D ( 'NONE', #10676, #11537, #11800 ) ;
#5393 = CARTESIAN_POINT ( 'NONE',  ( -8.162011110625947197, -94.39444938872335911, -1.717892133943179411 ) ) ;
#5394 = DIRECTION ( 'NONE',  ( 1.000000000000000000, 0.000000000000000000, 0.000000000000000000 ) ) ;
#5395 = EDGE_CURVE ( 'NONE', #4673, #12017, #5665, .T. ) ;
#5396 = ORIENTED_EDGE ( 'NONE', *, *, #5375, .F. ) ;
#5397 = VERTEX_POINT ( 'NONE', #3485 ) ;
#5398 = EDGE_CURVE ( 'NONE', #5054, #11019, #3198, .T. ) ;
#5399 = ADVANCED_FACE ( 'NONE', ( #12987 ), #9745, .F. ) ;
#5400 = PRODUCT_DEFINITION_SHAPE ( 'NONE', 'NONE',  #11145 ) ;
#5401 = CIRCLE ( 'NONE', #4974, 8.385254915620294014 ) ;
#5402 = DIRECTION ( 'NONE',  ( -6.158143864569485777E-17, -2.736152283717910599E-16, 1.000000000000000000 ) ) ;
#5403 = VERTEX_POINT ( 'NONE', #2369 ) ;
#5404 = DIRECTION ( 'NONE',  ( -0.9960067511297463483, 0.08927794634716618161, -4.818676322152979407E-17 ) ) ;
#5405 = CARTESIAN_POINT ( 'NONE',  ( -2.517691654963332357E-15, 90.00000000000000000, -1.589271161308885878E-16 ) ) ;
#5406 = FACE_OUTER_BOUND ( 'NONE', #12993, .T. ) ;
#5407 = CARTESIAN_POINT ( 'NONE',  ( 22.00000000000002132, -97.00000000000000000, 7.500000000000000000 ) ) ;
#5408 = CARTESIAN_POINT ( 'NONE',  ( -2.301581772533134895, -133.0909090909001975, 3.282526544929068812 ) ) ;
#5409 = CARTESIAN_POINT ( 'NONE',  ( 53.56517978609545594, 2.618988451796027572, 2.500000000000001776 ) ) ;
#5410 = CARTESIAN_POINT ( 'NONE',  ( -9.987599105575617031, -70.00000000000054001, -0.7388069302715789544 ) ) ;
#5411 = CARTESIAN_POINT ( 'NONE',  ( 1.463793564955054638, -80.12121212121228098, -10.07802918118900237 ) ) ;
#5412 = LINE ( 'NONE', #7719, #10544 ) ;
#5413 = DIRECTION ( 'NONE',  ( 0.7533101279583153120, -0.6576654553155628635, -1.445602896645893822E-16 ) ) ;
#5414 = ORIENTED_EDGE ( 'NONE', *, *, #2310, .T. ) ;
#5415 = ADVANCED_FACE ( 'NONE', ( #4334 ), #3355, .T. ) ;
#5416 = CARTESIAN_POINT ( 'NONE',  ( 16.53267785980283477, 10.29504797295195750, -2.499999999999997335 ) ) ;
#5417 = CARTESIAN_POINT ( 'NONE',  ( -8.385254915620292238, 71.87811454074363837, -2.234780678013320345E-15 ) ) ;
#5418 = ORIENTED_EDGE ( 'NONE', *, *, #12510, .F. ) ;
#5419 = DIRECTION ( 'NONE',  ( 0.000000000000000000, 0.000000000000000000, 1.000000000000000000 ) ) ;
#5420 = CARTESIAN_POINT ( 'NONE',  ( -25.00000000000000355, 120.0000000000000142, -2.500000000000000000 ) ) ;
#5421 = CARTESIAN_POINT ( 'NONE',  ( -15.29705854078138927, 90.00000000000000000, -1.589271161308885878E-16 ) ) ;
#5422 = ORIENTED_EDGE ( 'NONE', *, *, #6956, .F. ) ;
#5423 = CARTESIAN_POINT ( 'NONE',  ( -60.00000000000001421, 20.00000000000000000, 4.000000000000000000 ) ) ;
#5424 = DIRECTION ( 'NONE',  ( 0.000000000000000000, 0.000000000000000000, 1.000000000000000000 ) ) ;
#5425 = DIRECTION ( 'NONE',  ( 1.000000000000000000, 0.000000000000000000, 0.000000000000000000 ) ) ;
#5426 = CYLINDRICAL_SURFACE ( 'NONE', #1586, 8.385254915620294014 ) ;
#5427 = CARTESIAN_POINT ( 'NONE',  ( -15.29705854078139282, 27.21102387199583816, -3.793083824326958666E-15 ) ) ;
#5428 = CARTESIAN_POINT ( 'NONE',  ( 40.34010237645983921, 100.7894366958197594, 1.747896926826554731 ) ) ;
#5429 = CARTESIAN_POINT ( 'NONE',  ( -15.29705854078139105, 76.22148119144830503, -1.345962243664627229E-16 ) ) ;
#5430 = CIRCLE ( 'NONE', #13316, 25.00000000000000355 ) ;
#5431 = CARTESIAN_POINT ( 'NONE',  ( -12.99579180576516535, 16.95961992694555676, -1.651422005635246569E-15 ) ) ;
#5432 = VECTOR ( 'NONE', #6493, 1000.000000000000000 ) ;
#5433 = EDGE_CURVE ( 'NONE', #1229, #8596, #9578, .T. ) ;
#5434 = ORIENTED_EDGE ( 'NONE', *, *, #1830, .F. ) ;
#5435 = CIRCLE ( 'NONE', #1867, 15.00000000000000000 ) ;
#5436 = AXIS2_PLACEMENT_3D ( 'NONE', #6315, #12775, #9342 ) ;
#5437 = EDGE_LOOP ( 'NONE', ( #11086, #4869, #9506, #798 ) ) ;
#5438 = AXIS2_PLACEMENT_3D ( 'NONE', #7498, #11780, #4946 ) ;
#5439 = ORIENTED_EDGE ( 'NONE', *, *, #12038, .F. ) ;
#5440 = FACE_OUTER_BOUND ( 'NONE', #12531, .T. ) ;
#5441 = CARTESIAN_POINT ( 'NONE',  ( 10.69381717166374912, 53.83378072214353693, 21.38763434332751245 ) ) ;
#5442 = CARTESIAN_POINT ( 'NONE',  ( -19.02348910326480436, 26.95332645987220133, 6.306009631028898887 ) ) ;
#5443 = DIRECTION ( 'NONE',  ( -0.000000000000000000, -0.000000000000000000, -1.000000000000000000 ) ) ;
#5444 = B_SPLINE_CURVE_WITH_KNOTS ( 'NONE', 3,
 ( #446, #2610, #590, #8917, #4856, #8012, #1695, #2817, #12426, #6048, #8992, #10114, #9130, #4634, #6884, #1549, #5834, #13447, #3794, #5983, #12364, #2748, #7021, #10248, #9199, #13524, #3863, #12577 ),
 .UNSPECIFIED., .F., .F.,
 ( 4, 2, 2, 2, 2, 2, 2, 2, 2, 2, 2, 2, 2, 4 ),
 ( 0.000000000000000000, 0.002162634748517545339, 0.003243952122776318225, 0.004325269497035090678, 0.006487904245552661604, 0.008650538994070231663, 0.009731856368329017126, 0.01081317374258780085, 0.01189449111684658458, 0.01297580849110537005, 0.01513844323962291322, 0.01621976061388167439, 0.01676041930101106539, 0.01730107798814045639 ),
 .UNSPECIFIED. ) ;
#5445 = AXIS2_PLACEMENT_3D ( 'NONE', #5762, #13150, #4786 ) ;
#5446 = CARTESIAN_POINT ( 'NONE',  ( 12.99553232110413248, 11.07475474455194053, 25.99106464220827561 ) ) ;
#5447 = AXIS2_PLACEMENT_3D ( 'NONE', #5544, #3736, #7027 ) ;
#5448 = ORIENTED_EDGE ( 'NONE', *, *, #4190, .T. ) ;
#5449 = ORIENTED_EDGE ( 'NONE', *, *, #5159, .T. ) ;
#5450 = EDGE_CURVE ( 'NONE', #1473, #11569, #7767, .T. ) ;
#5451 = ORIENTED_EDGE ( 'NONE', *, *, #9124, .F. ) ;
#5452 = CARTESIAN_POINT ( 'NONE',  ( -15.29705854078139105, 76.22148119144830503, -3.882960684162827838E-15 ) ) ;
#5453 = ORIENTED_EDGE ( 'NONE', *, *, #13773, .T. ) ;
#5454 = CARTESIAN_POINT ( 'NONE',  ( 10.69381717166375267, 72.68333662216238622, 2.619229793989003556E-15 ) ) ;
#5455 = VECTOR ( 'NONE', #11959, 1000.000000000000000 ) ;
#5456 = DIRECTION ( 'NONE',  ( -2.797435172181481150E-17, 1.000000000000000000, -1.765856845898762549E-18 ) ) ;
#5457 = FILL_AREA_STYLE ('',( #288 ) ) ;
#5458 = CARTESIAN_POINT ( 'NONE',  ( -34.58461996471805122, 107.3565440455617903, -2.151643583074648536 ) ) ;
#5459 = CARTESIAN_POINT ( 'NONE',  ( 42.16244658108818300, 105.4500712252157655, 2.499999999999999556 ) ) ;
#5460 = CARTESIAN_POINT ( 'NONE',  ( -8.385254915620292238, 62.45333659073423860, -1.102836519679677113E-16 ) ) ;
#5461 = FACE_OUTER_BOUND ( 'NONE', #12425, .T. ) ;
#5462 = ORIENTED_EDGE ( 'NONE', *, *, #7650, .F. ) ;
#5463 = VERTEX_POINT ( 'NONE', #6726 ) ;
#5464 = EDGE_LOOP ( 'NONE', ( #179, #4010, #8731, #6372 ) ) ;
#5465 = CIRCLE ( 'NONE', #7946, 77.99999999999997158 ) ;
#5466 = EDGE_CURVE ( 'NONE', #4467, #3741, #10996, .T. ) ;
#5467 = AXIS2_PLACEMENT_3D ( 'NONE', #323, #13245, #10059 ) ;
#5468 = FACE_OUTER_BOUND ( 'NONE', #7722, .T. ) ;
#5469 = EDGE_CURVE ( 'NONE', #7762, #7874, #562, .T. ) ;
#5470 = DIRECTION ( 'NONE',  ( 1.000000000000000000, 0.000000000000000000, 0.000000000000000000 ) ) ;
#5471 = VERTEX_POINT ( 'NONE', #7339 ) ;
#5472 = CARTESIAN_POINT ( 'NONE',  ( 12.99579180576516713, -1.889935973073297859, 3.183050967463142591E-15 ) ) ;
#5473 = PRESENTATION_STYLE_ASSIGNMENT (( #2316 ) ) ;
#5474 = DIRECTION ( 'NONE',  ( 1.000000000000000000, 0.000000000000000000, 0.000000000000000000 ) ) ;
#5475 = CARTESIAN_POINT ( 'NONE',  ( 8.385254915620292238, 5.904668890677672088, 1.018788103988028800E-15 ) ) ;
#5476 = CARTESIAN_POINT ( 'NONE',  ( -3.039669588831499514, -137.4545454544692973, 0.1626128505621707299 ) ) ;
#5477 = LINE ( 'NONE', #6744, #714 ) ;
#5478 = CARTESIAN_POINT ( 'NONE',  ( -1.134746186792450207, -154.2164502169000855, -0.2399094883757922347 ) ) ;
#5479 = CARTESIAN_POINT ( 'NONE',  ( -9.314636722532608104, -70.78787878787781551, -4.145366960882149954 ) ) ;
#5480 = CARTESIAN_POINT ( 'NONE',  ( 8.385254915620292238, -15.56949922734665748, 16.77050983124059158 ) ) ;
#5481 = CARTESIAN_POINT ( 'NONE',  ( 35.00000000000000711, -25.00000000000000000, 4.000000000000000000 ) ) ;
#5482 = ORIENTED_EDGE ( 'NONE', *, *, #11006, .T. ) ;
#5483 = CARTESIAN_POINT ( 'NONE',  ( 42.70768697973989703, 17.09141780026012114, -2.499999999999993783 ) ) ;
#5484 = DIRECTION ( 'NONE',  ( -9.860761315262647568E-32, -3.204747427460360459E-31, 1.000000000000000000 ) ) ;
#5485 = ORIENTED_EDGE ( 'NONE', *, *, #5375, .T. ) ;
#5486 = AXIS2_PLACEMENT_3D ( 'NONE', #12160, #2769, #3668 ) ;
#5487 = ADVANCED_FACE ( 'NONE', ( #7279 ), #12396, .T. ) ;
#5488 = DIRECTION ( 'NONE',  ( -6.158143864569485777E-17, -2.736152283717910599E-16, 1.000000000000000000 ) ) ;
#5489 = PRESENTATION_LAYER_ASSIGNMENT (  '', '', ( #1702 ) ) ;
#5490 = EDGE_CURVE ( 'NONE', #6441, #6908, #9913, .T. ) ;
#5491 = CARTESIAN_POINT ( 'NONE',  ( 25.00000000000000355, 120.0000000000000142, -0.5000000000000000000 ) ) ;
#5492 = ORIENTED_EDGE ( 'NONE', *, *, #3025, .T. ) ;
#5493 = DIRECTION ( 'NONE',  ( -1.000000000000000000, 0.000000000000000000, 0.000000000000000000 ) ) ;
#5494 = ORIENTED_EDGE ( 'NONE', *, *, #8583, .F. ) ;
#5495 = CIRCLE ( 'NONE', #8625, 48.00000000000001421 ) ;
#5496 = CARTESIAN_POINT ( 'NONE',  ( -13.79311422413708499, -100.0000000000000000, -7.500000000000000000 ) ) ;
#5497 = FACE_OUTER_BOUND ( 'NONE', #13862, .T. ) ;
#5498 = ADVANCED_FACE ( 'NONE', ( #9396 ), #3206, .F. ) ;
#5499 = CARTESIAN_POINT ( 'NONE',  ( 25.00000000000000355, 120.0000000000000142, -0.5000000000000000000 ) ) ;
#5500 = ADVANCED_FACE ( 'NONE', ( #8467 ), #3136, .T. ) ;
#5501 = DIRECTION ( 'NONE',  ( 1.000000000000000000, 0.000000000000000000, 0.000000000000000000 ) ) ;
#5502 = DIRECTION ( 'NONE',  ( -0.000000000000000000, -0.000000000000000000, -1.000000000000000000 ) ) ;
#5503 = DIRECTION ( 'NONE',  ( -6.158143864569485777E-17, -2.736152283717910599E-16, 1.000000000000000000 ) ) ;
#5504 = AXIS2_PLACEMENT_3D ( 'NONE', #11515, #858, #3029 ) ;
#5505 = CARTESIAN_POINT ( 'NONE',  ( 9.847276892489302169E-17, -3.520109059331727686, 6.216008680731233110E-18 ) ) ;
#5506 = CARTESIAN_POINT ( 'NONE',  ( 25.00000000000000355, 120.0000000000000142, -7.500000000000000000 ) ) ;
#5507 = STYLED_ITEM ( 'NONE', ( #6363 ), #3546 ) ;
#5508 = DIRECTION ( 'NONE',  ( 0.000000000000000000, 0.000000000000000000, -1.000000000000000000 ) ) ;
#5509 = ORIENTED_EDGE ( 'NONE', *, *, #13517, .T. ) ;
#5510 = ORIENTED_EDGE ( 'NONE', *, *, #5359, .F. ) ;
#5511 = ORIENTED_EDGE ( 'NONE', *, *, #6851, .F. ) ;
#5512 = DIRECTION ( 'NONE',  ( -6.158143864569485777E-17, -2.736152283717910599E-16, 1.000000000000000000 ) ) ;
#5513 = EDGE_CURVE ( 'NONE', #12017, #12373, #6108, .T. ) ;
#5514 = CARTESIAN_POINT ( 'NONE',  ( 12.99579180576516002, 54.65873172698324112, 25.99158361153033425 ) ) ;
#5515 = DIRECTION ( 'NONE',  ( 1.000000000000000000, 0.000000000000000000, 0.000000000000000000 ) ) ;
#5516 = AXIS2_PLACEMENT_3D ( 'NONE', #694, #1800, #2856 ) ;
#5517 = FACE_BOUND ( 'NONE', #8418, .T. ) ;
#5518 = VERTEX_POINT ( 'NONE', #9663 ) ;
#5519 = PRODUCT_DEFINITION_SHAPE ( 'NONE', 'NONE',  #13899 ) ;
#5520 = VERTEX_POINT ( 'NONE', #2153 ) ;
#5521 = ORIENTED_EDGE ( 'NONE', *, *, #13254, .T. ) ;
#5522 = DIRECTION ( 'NONE',  ( 1.601283208593975514E-16, -1.000000000000000000, 0.000000000000000000 ) ) ;
#5523 = VERTEX_POINT ( 'NONE', #348 ) ;
#5524 = CARTESIAN_POINT ( 'NONE',  ( -1.024862805779478135E-15, 36.63580182200523438, -6.469358145237827718E-17 ) ) ;
#5525 = CARTESIAN_POINT ( 'NONE',  ( 0.9875500501441598633, -80.00464164738322381, -10.06307372056550342 ) ) ;
#5526 = DIRECTION ( 'NONE',  ( -2.797435172181481150E-17, 1.000000000000000000, -1.765856845898762549E-18 ) ) ;
#5527 = CARTESIAN_POINT ( 'NONE',  ( 4.267662252619970786, 91.33687515530506573, -2.605658972705547249 ) ) ;
#5528 = CARTESIAN_POINT ( 'NONE',  ( 15.29705854078140348, -29.33764382806072746, 1.980000072520088949E-15 ) ) ;
#5529 = DIRECTION ( 'NONE',  ( 1.000000000000000000, -0.000000000000000000, -0.000000000000000000 ) ) ;
#5530 = ORIENTED_EDGE ( 'NONE', *, *, #5903, .T. ) ;
#5531 = CIRCLE ( 'NONE', #5309, 69.99999999999998579 ) ;
#5532 = ORIENTED_EDGE ( 'NONE', *, *, #7281, .T. ) ;
#5533 = ORIENTED_EDGE ( 'NONE', *, *, #1284, .F. ) ;
#5534 = CARTESIAN_POINT ( 'NONE',  ( -4.330127018922195425, 92.00000000000000000, 2.500000000000000000 ) ) ;
#5535 = ORIENTED_EDGE ( 'NONE', *, *, #3869, .T. ) ;
#5536 = CARTESIAN_POINT ( 'NONE',  ( 34.99999999999999289, 25.00000000000002132, -7.500000000000000000 ) ) ;
#5537 = DIRECTION ( 'NONE',  ( 0.6466635011015214873, -0.7627754036039198215, 3.014552924381575957E-15 ) ) ;
#5538 = FACE_OUTER_BOUND ( 'NONE', #13307, .T. ) ;
#5539 = DIRECTION ( 'NONE',  ( -1.000000000000000000, 0.000000000000000000, 0.000000000000000000 ) ) ;
#5540 = CARTESIAN_POINT ( 'NONE',  ( -0.8539417517645131461, -80.00115723678993618, -9.969673860083380745 ) ) ;
#5541 = CARTESIAN_POINT ( 'NONE',  ( 1.214590548353038368, -168.0000000000000568, -1.662759693958060225 ) ) ;
#5542 = CARTESIAN_POINT ( 'NONE',  ( 0.2617580721754693696, -80.12121212121134306, -10.03731802028341136 ) ) ;
#5543 = CARTESIAN_POINT ( 'NONE',  ( 10.99999999999999289, 147.0000000000000284, 7.500000000000000000 ) ) ;
#5544 = CARTESIAN_POINT ( 'NONE',  ( 55.00383357371546822, 6.846651893462920135, -2.499999999999995559 ) ) ;
#5545 = EDGE_CURVE ( 'NONE', #11430, #8708, #2290, .T. ) ;
#5546 = AXIS2_PLACEMENT_3D ( 'NONE', #2618, #9273, #11096 ) ;
#5547 = ORIENTED_EDGE ( 'NONE', *, *, #1889, .T. ) ;
#5548 = CIRCLE ( 'NONE', #1752, 25.50000000002549783 ) ;
#5549 = CARTESIAN_POINT ( 'NONE',  ( -35.00000000000000000, -4.286263797015736496E-15, 7.500000000000000000 ) ) ;
#5550 = ORIENTED_EDGE ( 'NONE', *, *, #8419, .F. ) ;
#5551 = DIRECTION ( 'NONE',  ( -0.2228746399763467390, 0.9748471135800802490, 2.409338161076489210E-16 ) ) ;
#5552 = CYLINDRICAL_SURFACE ( 'NONE', #1588, 8.385254915620295790 ) ;
#5553 = ORIENTED_EDGE ( 'NONE', *, *, #9317, .F. ) ;
#5554 = CARTESIAN_POINT ( 'NONE',  ( -8.385254915620292238, 5.904668890677672088, -1.042679998336861873E-17 ) ) ;
#5555 = ORIENTED_EDGE ( 'NONE', *, *, #6202, .F. ) ;
#5556 = CARTESIAN_POINT ( 'NONE',  ( -37.50000000000000711, -4.286263797015736496E-15, 7.500000000000000000 ) ) ;
#5557 = VECTOR ( 'NONE', #1036, 1000.000000000000000 ) ;
#5558 = CARTESIAN_POINT ( 'NONE',  ( -15.29705854078139282, 27.21102387199583816, -1.969450923410318186E-15 ) ) ;
#5559 = ADVANCED_BREP_SHAPE_REPRESENTATION ( '', ( #7994, #8193 ), #13606 ) ;
#5560 = DIRECTION ( 'NONE',  ( -0.000000000000000000, -0.000000000000000000, -1.000000000000000000 ) ) ;
#5561 = CARTESIAN_POINT ( 'NONE',  ( -1.341290363786561812E-15, 47.94714734142005597, -8.466779837416320124E-17 ) ) ;
#5562 = CARTESIAN_POINT ( 'NONE',  ( -15.29705854078138216, 10.24803554138234318, -30.59411708156277498 ) ) ;
#5563 = CARTESIAN_POINT ( 'NONE',  ( -10.69381717166376156, -30.98922082794128130, -1.200169841498325292E-15 ) ) ;
#5564 = DIRECTION ( 'NONE',  ( 0.9928035427100113663, 0.1197544386753605777, 9.252351997306908241E-17 ) ) ;
#5565 = EDGE_CURVE ( 'NONE', #2097, #11234, #1402, .T. ) ;
#5566 = CARTESIAN_POINT ( 'NONE',  ( 1.958204620527036497E-15, -70.00000000000000000, 1.236099792129133461E-16 ) ) ;
#5567 = EDGE_CURVE ( 'NONE', #10692, #2953, #12602, .T. ) ;
#5568 = EDGE_CURVE ( 'NONE', #12557, #11359, #11025, .T. ) ;
#5569 = ORIENTED_EDGE ( 'NONE', *, *, #6532, .F. ) ;
#5570 = AXIS2_PLACEMENT_3D ( 'NONE', #2384, #2319, #6598 ) ;
#5571 = ORIENTED_EDGE ( 'NONE', *, *, #1219, .F. ) ;
#5572 = EDGE_CURVE ( 'NONE', #2860, #4027, #4524, .T. ) ;
#5573 = EDGE_CURVE ( 'NONE', #3719, #1421, #6640, .T. ) ;
#5574 = CIRCLE ( 'NONE', #4915, 9.000000000008999024 ) ;
#5575 =( BOUNDED_SURFACE ( )  B_SPLINE_SURFACE ( 3, 3, ( 
 ( #2359, #10834, #7548, #9874 ),
 ( #10904, #11765, #3406, #278 ),
 ( #2221, #9594, #5446, #1253 ),
 ( #1116, #4256, #8674, #6508 ) ),
 .UNSPECIFIED., .F., .F., .T. ) 
 B_SPLINE_SURFACE_WITH_KNOTS ( ( 4, 4 ),
 ( 4, 4 ),
 ( 0.000000000000000000, 1.000000000000000000 ),
 ( 0.000000000000000000, 1.000000000000000000 ),
 .UNSPECIFIED. ) 
 GEOMETRIC_REPRESENTATION_ITEM ( )  RATIONAL_B_SPLINE_SURFACE ( (
 ( 1.000000000000000000, 0.3333333333333334259, 0.3333333333333334259, 1.000000000000000000),
 ( 1.000000000000000000, 0.3333333333333334259, 0.3333333333333334259, 1.000000000000000000),
 ( 1.000000000000000000, 0.3333333333333334259, 0.3333333333333334259, 1.000000000000000000),
 ( 1.000000000000000000, 0.3333333333333334259, 0.3333333333333334259, 1.000000000000000000) ) ) 
 REPRESENTATION_ITEM ( '' )  SURFACE ( )  );
#5576 = ORIENTED_EDGE ( 'NONE', *, *, #1952, .F. ) ;
#5577 = DIRECTION ( 'NONE',  ( 0.000000000000000000, 0.000000000000000000, 1.000000000000000000 ) ) ;
#5578 = APPLICATION_PROTOCOL_DEFINITION ( 'draft international standard', 'automotive_design', 1998, #10065 ) ;
#5579 = VERTEX_POINT ( 'NONE', #3474 ) ;
#5580 = DIRECTION ( 'NONE',  ( -0.000000000000000000, -0.000000000000000000, -1.000000000000000000 ) ) ;
#5581 = CIRCLE ( 'NONE', #2225, 5.999999999999998224 ) ;
#5582 = CARTESIAN_POINT ( 'NONE',  ( 25.00000000000001421, -99.72710464630424099, 4.238242954203321311 ) ) ;
#5583 = DIRECTION ( 'NONE',  ( -0.7328050451781167318, -0.6804386568688601811, -2.313087999326727184E-16 ) ) ;
#5584 = VECTOR ( 'NONE', #4361, 1000.000000000000000 ) ;
#5585 = CARTESIAN_POINT ( 'NONE',  ( 45.97632359910777922, 102.2167537197081657, 2.499999999999999556 ) ) ;
#5586 = EDGE_LOOP ( 'NONE', ( #11772, #2609, #11900, #1390 ) ) ;
#5587 = VERTEX_POINT ( 'NONE', #1308 ) ;
#5588 = ADVANCED_FACE ( 'NONE', ( #4607 ), #9873, .T. ) ;
#5589 = CIRCLE ( 'NONE', #5150, 8.385254915620294014 ) ;
#5590 = CARTESIAN_POINT ( 'NONE',  ( 35.04450421339217314, 112.5597086678580609, 7.500000000000000000 ) ) ;
#5591 = CIRCLE ( 'NONE', #13494, 4.999999999999997335 ) ;
#5592 = AXIS2_PLACEMENT_3D ( 'NONE', #12708, #8417, #7348 ) ;
#5593 = ORIENTED_EDGE ( 'NONE', *, *, #5398, .F. ) ;
#5594 = VERTEX_POINT ( 'NONE', #3543 ) ;
#5595 = DIRECTION ( 'NONE',  ( 0.1234677578012386701, 0.000000000000000000, -0.9923485843107424653 ) ) ;
#5596 = ORIENTED_EDGE ( 'NONE', *, *, #11995, .T. ) ;
#5597 = DIRECTION ( 'NONE',  ( -6.158143864569485777E-17, -2.736152283717910599E-16, 1.000000000000000000 ) ) ;
#5598 = DIRECTION ( 'NONE',  ( 0.000000000000000000, -1.000000000000000000, 0.000000000000000000 ) ) ;
#5599 = CARTESIAN_POINT ( 'NONE',  ( -35.00000000000012079, 91.25000000000045475, 7.500000000000000000 ) ) ;
#5600 = DIRECTION ( 'NONE',  ( 1.000000000000000000, 0.000000000000000000, 0.000000000000000000 ) ) ;
#5601 = DIRECTION ( 'NONE',  ( -2.797435172181481150E-17, 1.000000000000000000, -1.765856845898762549E-18 ) ) ;
#5602 = AXIS2_PLACEMENT_3D ( 'NONE', #12805, #5083, #6338 ) ;
#5603 = CARTESIAN_POINT ( 'NONE',  ( 10.69381717166376333, -30.98922082794128130, 1.384171912460316962E-15 ) ) ;
#5604 = DIRECTION ( 'NONE',  ( 0.000000000000000000, 0.000000000000000000, 1.000000000000000000 ) ) ;
#5605 = ORIENTED_EDGE ( 'NONE', *, *, #13221, .T. ) ;
#5606 = AXIS2_PLACEMENT_3D ( 'NONE', #2701, #10339, #6975 ) ;
#5607 = VERTEX_POINT ( 'NONE', #13196 ) ;
#5608 = ORIENTED_EDGE ( 'NONE', *, *, #2673, .F. ) ;
#5609 = CARTESIAN_POINT ( 'NONE',  ( -8.713593516913357817, -91.08576818318459800, -0.8596443958658561701 ) ) ;
#5610 = ADVANCED_FACE ( 'NONE', ( #7754 ), #8888, .F. ) ;
#5611 = CARTESIAN_POINT ( 'NONE',  ( -3.828023344975119979, 90.45717703472959670, 3.219997411495244322 ) ) ;
#5612 = AXIS2_PLACEMENT_3D ( 'NONE', #1216, #13009, #12003 ) ;
#5613 = CARTESIAN_POINT ( 'NONE',  ( -37.50000000000002132, 144.4948974278317735, 2.499999999999999556 ) ) ;
#5614 = EDGE_LOOP ( 'NONE', ( #11627, #210, #7003, #2810 ) ) ;
#5615 = DIRECTION ( 'NONE',  ( -1.000000000000000000, 0.000000000000000000, 0.000000000000000000 ) ) ;
#5616 = CARTESIAN_POINT ( 'NONE',  ( 10.69381717166375445, 34.98422482212468054, 2.619229793989003951E-15 ) ) ;
#5617 = CARTESIAN_POINT ( 'NONE',  ( -12.99553232110414491, -7.774801155466915858, -3.169847907505149691E-15 ) ) ;
#5618 = AXIS2_PLACEMENT_3D ( 'NONE', #7104, #10402, #12721 ) ;
#5619 = DIRECTION ( 'NONE',  ( 1.000000000000000000, 0.000000000000000000, 0.000000000000000000 ) ) ;
#5620 = CARTESIAN_POINT ( 'NONE',  ( -0.3237100442214350671, -158.0606060598179283, -0.5247744424615701231 ) ) ;
#5621 = FACE_OUTER_BOUND ( 'NONE', #1058, .T. ) ;
#5622 = CARTESIAN_POINT ( 'NONE',  ( -27.38873514654796537, -24.33759740261775661, -4.000000000000000000 ) ) ;
#5623 = CARTESIAN_POINT ( 'NONE',  ( -25.00000000000000355, 120.0000000000000142, -7.500000000000000000 ) ) ;
#5624 = ORIENTED_EDGE ( 'NONE', *, *, #11526, .T. ) ;
#5625 = ORIENTED_EDGE ( 'NONE', *, *, #10382, .F. ) ;
#5626 = AXIS2_PLACEMENT_3D ( 'NONE', #8034, #809, #12245 ) ;
#5627 = LINE ( 'NONE', #9986, #472 ) ;
#5628 = FACE_BOUND ( 'NONE', #10366, .T. ) ;
#5629 = CARTESIAN_POINT ( 'NONE',  ( -24.99999999999998934, -99.24349759607916610, -1.707585965103561865 ) ) ;
#5630 = DIRECTION ( 'NONE',  ( -1.000000000000000000, 0.000000000000000000, 0.000000000000000000 ) ) ;
#5631 = ORIENTED_EDGE ( 'NONE', *, *, #6703, .F. ) ;
#5632 = VERTEX_POINT ( 'NONE', #12910 ) ;
#5633 = CARTESIAN_POINT ( 'NONE',  ( 4.330127018922190985, 90.00000000000000000, -4.500000000000000888 ) ) ;
#5634 = ORIENTED_EDGE ( 'NONE', *, *, #1897, .F. ) ;
#5635 = DIRECTION ( 'NONE',  ( -1.000000000000000000, 0.000000000000000000, 0.000000000000000000 ) ) ;
#5636 = ADVANCED_FACE ( 'NONE', ( #7547 ), #205, .T. ) ;
#5637 = CARTESIAN_POINT ( 'NONE',  ( -15.29705854078139105, 27.21102387199583816, -4.805077278827845308E-17 ) ) ;
#5638 = CARTESIAN_POINT ( 'NONE',  ( -12.99579180576516713, 45.23395377697384134, -3.272288958712398313E-15 ) ) ;
#5639 = FACE_OUTER_BOUND ( 'NONE', #10808, .T. ) ;
#5640 =( BOUNDED_SURFACE ( )  B_SPLINE_SURFACE ( 3, 3, ( 
 ( #9429, #10539, #11661, #13741 ),
 ( #944, #12663, #10671, #36 ),
 ( #6334, #5343, #13805, #9628 ),
 ( #4154, #3043, #5207, #8438 ) ),
 .UNSPECIFIED., .F., .F., .T. ) 
 B_SPLINE_SURFACE_WITH_KNOTS ( ( 4, 4 ),
 ( 4, 4 ),
 ( 0.000000000000000000, 1.000000000000000000 ),
 ( 0.000000000000000000, 1.000000000000000000 ),
 .UNSPECIFIED. ) 
 GEOMETRIC_REPRESENTATION_ITEM ( )  RATIONAL_B_SPLINE_SURFACE ( (
 ( 1.000000000000000000, 0.3333333333333334259, 0.3333333333333334259, 1.000000000000000000),
 ( 1.000000000000000000, 0.3333333333333334259, 0.3333333333333334259, 1.000000000000000000),
 ( 1.000000000000000000, 0.3333333333333334259, 0.3333333333333334259, 1.000000000000000000),
 ( 1.000000000000000000, 0.3333333333333334259, 0.3333333333333334259, 1.000000000000000000) ) ) 
 REPRESENTATION_ITEM ( '' )  SURFACE ( )  );
#5641 = DIRECTION ( 'NONE',  ( -2.797435172181481150E-17, 1.000000000000000000, -1.765856845898762549E-18 ) ) ;
#5642 = DIRECTION ( 'NONE',  ( -2.797435172181479917E-17, 1.000000000000000000, -1.765856845898779112E-18 ) ) ;
#5643 = CARTESIAN_POINT ( 'NONE',  ( -8.385254915620294014, -31.79444290936001138, -9.146086898988387700E-16 ) ) ;
#5644 = CARTESIAN_POINT ( 'NONE',  ( 34.99999999999958789, 1.063887963769481123E-13, 12.50000000000000000 ) ) ;
#5645 = CARTESIAN_POINT ( 'NONE',  ( 14.00979921278056040, -2.538005261501628862, 2.499999999999997780 ) ) ;
#5646 = ORIENTED_EDGE ( 'NONE', *, *, #7631, .F. ) ;
#5647 = CARTESIAN_POINT ( 'NONE',  ( -1.651792843486753513E-16, 5.904668890677672088, -1.042679998336861873E-17 ) ) ;
#5648 = VERTEX_POINT ( 'NONE', #9800 ) ;
#5649 = ORIENTED_EDGE ( 'NONE', *, *, #11273, .F. ) ;
#5650 = CARTESIAN_POINT ( 'NONE',  ( -8.385254915620294014, 3.280056672672198914, -5.792110530374064999E-18 ) ) ;
#5651 = EDGE_CURVE ( 'NONE', #214, #863, #6124, .T. ) ;
#5652 = CONTEXT_DEPENDENT_SHAPE_REPRESENTATION ( #13029, #10143 ) ;
#5653 = B_SPLINE_CURVE_WITH_KNOTS ( 'NONE', 3,
 ( #4670, #2713, #11196, #486, #619, #11045, #3898, #3685, #6773, #8957, #8041, #1589, #9157, #7970, #5720, #4879 ),
 .UNSPECIFIED., .F., .F.,
 ( 4, 2, 2, 2, 2, 2, 2, 4 ),
 ( 0.000000000000000000, 0.0005014865247272642327, 0.001002973049454528465, 0.001504459574181792698, 0.002005946098909056931, 0.002507432623636320947, 0.003008919148363585396, 0.004011892197818113862 ),
 .UNSPECIFIED. ) ;
#5654 = EDGE_CURVE ( 'NONE', #9893, #3489, #295, .T. ) ;
#5655 = ORIENTED_EDGE ( 'NONE', *, *, #2379, .F. ) ;
#5656 = DIRECTION ( 'NONE',  ( -0.6000000000000001998, -0.7999999999999998224, 0.000000000000000000 ) ) ;
#5657 = CARTESIAN_POINT ( 'NONE',  ( -40.05868326948371561, 100.9130297721161327, 2.014878269406402467 ) ) ;
#5658 = EDGE_CURVE ( 'NONE', #10679, #6325, #6782, .T. ) ;
#5659 = AXIS2_PLACEMENT_3D ( 'NONE', #7813, #11123, #4667 ) ;
#5660 = ADVANCED_FACE ( 'NONE', ( #10700 ), #6507, .T. ) ;
#5661 = DIRECTION ( 'NONE',  ( -1.000000000000000000, 0.000000000000000000, 0.000000000000000000 ) ) ;
#5662 = CARTESIAN_POINT ( 'NONE',  ( 7.521705593689169689, -75.41806776122028566, 6.778495972023521610 ) ) ;
#5663 = VERTEX_POINT ( 'NONE', #142 ) ;
#5664 = ORIENTED_EDGE ( 'NONE', *, *, #12704, .F. ) ;
#5665 = CIRCLE ( 'NONE', #7918, 18.74900000001875355 ) ;
#5666 = EDGE_CURVE ( 'NONE', #6479, #9684, #13082, .T. ) ;
#5667 = ORIENTED_EDGE ( 'NONE', *, *, #5736, .F. ) ;
#5668 = ORIENTED_EDGE ( 'NONE', *, *, #4188, .F. ) ;
#5669 = LINE ( 'NONE', #8860, #13249 ) ;
#5670 = EDGE_LOOP ( 'NONE', ( #7711, #9793, #2081, #468 ) ) ;
#5671 = CARTESIAN_POINT ( 'NONE',  ( 0.6173387890061953209, -69.99999999999998579, -4.961742921553712549 ) ) ;
#5672 = CIRCLE ( 'NONE', #5002, 2.000000000000003109 ) ;
#5673 = FACE_OUTER_BOUND ( 'NONE', #6247, .T. ) ;
#5674 = EDGE_CURVE ( 'NONE', #4194, #6463, #7907, .T. ) ;
#5675 = AXIS2_PLACEMENT_3D ( 'NONE', #3440, #10802, #40 ) ;
#5676 = CARTESIAN_POINT ( 'NONE',  ( -7.861734782780223085, -72.85454080786820441, -6.394819305376118201 ) ) ;
#5677 = EDGE_CURVE ( 'NONE', #2194, #2762, #7443, .T. ) ;
#5678 = CARTESIAN_POINT ( 'NONE',  ( -34.40224804986665674, 107.7695571918731758, 1.740729949763268447 ) ) ;
#5679 = CARTESIAN_POINT ( 'NONE',  ( -25.00000000000000000, -35.00000000000000000, 7.500000000000000000 ) ) ;
#5680 = CARTESIAN_POINT ( 'NONE',  ( 12.99553232110413781, 58.19864449459907974, 3.182987412051231773E-15 ) ) ;
#5681 = ORIENTED_EDGE ( 'NONE', *, *, #543, .T. ) ;
#5682 = ORIENTED_EDGE ( 'NONE', *, *, #8070, .F. ) ;
#5683 = CIRCLE ( 'NONE', #13354, 66.25000000000044054 ) ;
#5684 = DIRECTION ( 'NONE',  ( -0.000000000000000000, -0.000000000000000000, -1.000000000000000000 ) ) ;
#5685 = CARTESIAN_POINT ( 'NONE',  ( 21.51985683731163945, -13.03114504999992995, -2.500000000000004441 ) ) ;
#5686 = VERTEX_POINT ( 'NONE', #1672 ) ;
#5687 = DIRECTION ( 'NONE',  ( -6.158143864569485777E-17, -2.736152283717910599E-16, 1.000000000000000000 ) ) ;
#5688 = CARTESIAN_POINT ( 'NONE',  ( -15.29705854078138394, 57.37192529142944863, -30.59411708156277854 ) ) ;
#5689 = LINE ( 'NONE', #4561, #12180 ) ;
#5690 = CARTESIAN_POINT ( 'NONE',  ( 4.418010223187812890, -106.9090909090834742, -5.547116815808206702 ) ) ;
#5691 = DIRECTION ( 'NONE',  ( -6.158143864569485777E-17, -2.736152283717910599E-16, 1.000000000000000000 ) ) ;
#5692 = CARTESIAN_POINT ( 'NONE',  ( 3.189539364161639412, -137.4545454545230143, -1.430838129453004370 ) ) ;
#5693 = EDGE_CURVE ( 'NONE', #11449, #1592, #5430, .T. ) ;
#5694 = LINE ( 'NONE', #2617, #12683 ) ;
#5695 = VECTOR ( 'NONE', #6366, 1000.000000000000000 ) ;
#5696 = CARTESIAN_POINT ( 'NONE',  ( -15.29705854078139815, -18.02629830864593785, 30.59411708156277854 ) ) ;
#5697 = DIRECTION ( 'NONE',  ( -2.797435172181481150E-17, 1.000000000000000000, -1.765856845898762549E-18 ) ) ;
#5698 = CIRCLE ( 'NONE', #7482, 2.500000000000002220 ) ;
#5699 = ORIENTED_EDGE ( 'NONE', *, *, #3161, .F. ) ;
#5700 = ORIENTED_EDGE ( 'NONE', *, *, #8583, .T. ) ;
#5701 = VECTOR ( 'NONE', #11543, 1000.000000000000000 ) ;
#5702 = ORIENTED_EDGE ( 'NONE', *, *, #6899, .T. ) ;
#5703 = DIRECTION ( 'NONE',  ( -2.797435172181481150E-17, 1.000000000000000000, -1.765856845898762549E-18 ) ) ;
#5704 = VERTEX_POINT ( 'NONE', #10293 ) ;
#5706 = ORIENTED_EDGE ( 'NONE', *, *, #7517, .F. ) ;
#5705 = CIRCLE ( 'NONE', #5954, 71.99999999999998579 ) ;
#5707 = CYLINDRICAL_SURFACE ( 'NONE', #11310, 27.49999999999998934 ) ;
#5708 = VERTEX_POINT ( 'NONE', #12118 ) ;
#5709 = CARTESIAN_POINT ( 'NONE',  ( -39.00000000000000000, -3.796405077356795904E-15, 8.499999999999998224 ) ) ;
#5710 = CARTESIAN_POINT ( 'NONE',  ( 8.385254915620292238, 15.32944684068712782, 1.002145295323929148E-15 ) ) ;
#5711 = DIRECTION ( 'NONE',  ( -1.000000000000000000, 0.000000000000000000, 0.000000000000000000 ) ) ;
#5712 = B_SPLINE_CURVE_WITH_KNOTS ( 'NONE', 3,
 ( #1488, #7944, #12228, #10048, #10255, #6889, #4792, #9069, #11169, #12431, #3735, #8019 ),
 .UNSPECIFIED., .F., .F.,
 ( 4, 2, 2, 2, 2, 4 ),
 ( 0.000000000000000000, 0.002041637357698527708, 0.003062456036547791995, 0.004083274715397057150, 0.006124912073095585725, 0.008166549430794116035 ),
 .UNSPECIFIED. ) ;
#5713 = CARTESIAN_POINT ( 'NONE',  ( -10.69381717166376156, -30.98922082794128130, -1.200169841498325292E-15 ) ) ;
#5714 = CARTESIAN_POINT ( 'NONE',  ( -7.521705564882291029, -75.41806779423124851, -6.778496005277558467 ) ) ;
#5715 = CARTESIAN_POINT ( 'NONE',  ( 32.72727272727274084, 135.1423002281141805, 2.500000000000000000 ) ) ;
#5716 = CARTESIAN_POINT ( 'NONE',  ( -12.99553232110414136, -36.04913500549519512, -1.464178482349251183E-15 ) ) ;
#5717 = FACE_OUTER_BOUND ( 'NONE', #2512, .T. ) ;
#5718 = AXIS2_PLACEMENT_3D ( 'NONE', #9144, #13466, #13395 ) ;
#5719 = CARTESIAN_POINT ( 'NONE',  ( 10.00000000000000711, 139.9999999999999716, 2.500000000000000000 ) ) ;
#5720 = CARTESIAN_POINT ( 'NONE',  ( 2.482729886976819511, 90.00000000000001421, 4.353114590951097540 ) ) ;
#5721 = ORIENTED_EDGE ( 'NONE', *, *, #8673, .T. ) ;
#5722 = ADVANCED_BREP_SHAPE_REPRESENTATION ( '', ( #3316, #8193 ), #1690 ) ;
#5723 = AXIS2_PLACEMENT_3D ( 'NONE', #6585, #10785, #12927 ) ;
#5724 = VERTEX_POINT ( 'NONE', #9169 ) ;
#5725 = CARTESIAN_POINT ( 'NONE',  ( -31.81818181818181657, 133.3608531424536920, -0.5000000000000000000 ) ) ;
#5726 = ORIENTED_EDGE ( 'NONE', *, *, #271, .T. ) ;
#5727 = CARTESIAN_POINT ( 'NONE',  ( 5.042740091284176371E-16, -18.02629830864596627, 3.183186227453577089E-17 ) ) ;
#5728 = CARTESIAN_POINT ( 'NONE',  ( 12.99579180576516890, 64.08350967699263379, 0.000000000000000000 ) ) ;
#5729 = DIRECTION ( 'NONE',  ( 1.000000000000000000, 0.000000000000000000, 0.000000000000000000 ) ) ;
#5730 = CIRCLE ( 'NONE', #7984, 25.50000000002549783 ) ;
#5731 = DIRECTION ( 'NONE',  ( 2.797435172181480534E-17, -1.000000000000000000, 1.765856845898762164E-18 ) ) ;
#5732 = CARTESIAN_POINT ( 'NONE',  ( 4.918402716924989981, -70.00000000000000000, -0.8996192050778424321 ) ) ;
#5733 = EDGE_LOOP ( 'NONE', ( #6029, #6409, #1054, #647, #4966 ) ) ;
#5734 = EDGE_CURVE ( 'NONE', #3663, #7690, #10226, .T. ) ;
#5735 = EDGE_LOOP ( 'NONE', ( #8767, #10666 ) ) ;
#5736 = EDGE_CURVE ( 'NONE', #2504, #1229, #1186, .T. ) ;
#5737 = CIRCLE ( 'NONE', #11122, 22.99999999999999645 ) ;
#5738 = CARTESIAN_POINT ( 'NONE',  ( -25.00000000000000355, 120.0000000000000142, 7.500000000000000000 ) ) ;
#5739 = ORIENTED_EDGE ( 'NONE', *, *, #11843, .T. ) ;
#5740 = DIRECTION ( 'NONE',  ( 1.000000000000000000, 0.000000000000000000, 0.000000000000000000 ) ) ;
#5741 = TOROIDAL_SURFACE ( 'NONE', #394, 48.00000000000001421, 2.000000000000000000 ) ;
#5742 = CARTESIAN_POINT ( 'NONE',  ( 15.29705854078138572, 57.37192529142945574, 1.773704474924340342E-15 ) ) ;
#5743 = DIRECTION ( 'NONE',  ( 0.000000000000000000, 0.000000000000000000, 1.000000000000000000 ) ) ;
#5744 = CYLINDRICAL_SURFACE ( 'NONE', #13615, 25.50000000002550138 ) ;
#5745 = CARTESIAN_POINT ( 'NONE',  ( -0.9319787617451019690, -80.77036012704304824, -9.970313506240117363 ) ) ;
#5746 = FACE_OUTER_BOUND ( 'NONE', #10922, .T. ) ;
#5747 =( BOUNDED_SURFACE ( )  B_SPLINE_SURFACE ( 3, 3, ( 
 ( #5528, #9816, #221, #4478 ),
 ( #2446, #7701, #13132, #3486 ),
 ( #5603, #7768, #3715, #2665 ),
 ( #3853, #13511, #8135, #6803 ) ),
 .UNSPECIFIED., .F., .F., .T. ) 
 B_SPLINE_SURFACE_WITH_KNOTS ( ( 4, 4 ),
 ( 4, 4 ),
 ( 0.000000000000000000, 1.000000000000000000 ),
 ( 0.000000000000000000, 1.000000000000000000 ),
 .UNSPECIFIED. ) 
 GEOMETRIC_REPRESENTATION_ITEM ( )  RATIONAL_B_SPLINE_SURFACE ( (
 ( 1.000000000000000000, 0.3333333333333334259, 0.3333333333333334259, 1.000000000000000000),
 ( 1.000000000000000000, 0.3333333333333334259, 0.3333333333333334259, 1.000000000000000000),
 ( 1.000000000000000000, 0.3333333333333334259, 0.3333333333333334259, 1.000000000000000000),
 ( 1.000000000000000000, 0.3333333333333334259, 0.3333333333333334259, 1.000000000000000000) ) ) 
 REPRESENTATION_ITEM ( '' )  SURFACE ( )  );
#5748 = EDGE_CURVE ( 'NONE', #1913, #2762, #2770, .T. ) ;
#5749 = ORIENTED_EDGE ( 'NONE', *, *, #6079, .T. ) ;
#5750 = EDGE_CURVE ( 'NONE', #8935, #624, #4777, .T. ) ;
#5751 = EDGE_CURVE ( 'NONE', #5471, #6547, #12624, .T. ) ;
#5752 = CARTESIAN_POINT ( 'NONE',  ( -8.385254915620299343, -6.144721277337256815, 16.77050983124059158 ) ) ;
#5753 = EDGE_CURVE ( 'NONE', #2743, #4734, #2796, .T. ) ;
#5754 = ADVANCED_FACE ( 'NONE', ( #696 ), #9968, .T. ) ;
#5755 = PRODUCT_DEFINITION_SHAPE ( 'NONE', 'NONE',  #13904 ) ;
#5756 = CARTESIAN_POINT ( 'NONE',  ( -15.29705854078139815, -27.45107625865536960, 30.59411708156277854 ) ) ;
#5757 =( REPRESENTATION_RELATIONSHIP ('NONE','NONE', #9450, #3787 ) REPRESENTATION_RELATIONSHIP_WITH_TRANSFORMATION ( #10975 )SHAPE_REPRESENTATION_RELATIONSHIP( ) );
#5758 = CARTESIAN_POINT ( 'NONE',  ( 9.082088619475626956, -71.90909090908733958, 4.345719731624217985 ) ) ;
#5759 = ORIENTED_EDGE ( 'NONE', *, *, #4560, .F. ) ;
#5760 = CARTESIAN_POINT ( 'NONE',  ( 4.545447045960947285, 90.76293396533760927, 2.092248084982493594 ) ) ;
#5761 = FACE_OUTER_BOUND ( 'NONE', #12496, .T. ) ;
#5762 = CARTESIAN_POINT ( 'NONE',  ( 25.00000000000000355, 120.0000000000000142, -2.499999999999998668 ) ) ;
#5763 = FACE_BOUND ( 'NONE', #934, .T. ) ;
#5764 = CARTESIAN_POINT ( 'NONE',  ( 1.652786589946103835, -148.3982683981489856, 1.815848636690450268 ) ) ;
#5765 = CARTESIAN_POINT ( 'NONE',  ( 34.99999999999958789, 1.091249486606660213E-13, 2.500000000000000000 ) ) ;
#5766 = B_SPLINE_CURVE_WITH_KNOTS ( 'NONE', 3,
 ( #7734, #10953, #9781, #325 ),
 .UNSPECIFIED., .F., .F.,
 ( 4, 4 ),
 ( 0.02301878569831470461, 0.02656428146801016396 ),
 .UNSPECIFIED. ) ;
#5767 = DIRECTION ( 'NONE',  ( 0.9960067511297463483, -0.08927794634716618161, 4.818676322152979407E-17 ) ) ;
#5768 = SURFACE_SIDE_STYLE ('',( #12005 ) ) ;
#5769 = ORIENTED_EDGE ( 'NONE', *, *, #8067, .F. ) ;
#5770 = ORIENTED_EDGE ( 'NONE', *, *, #7290, .T. ) ;
#5771 = EDGE_CURVE ( 'NONE', #11226, #11483, #11928, .T. ) ;
#5772 = ORIENTED_EDGE ( 'NONE', *, *, #10551, .F. ) ;
#5773 = CARTESIAN_POINT ( 'NONE',  ( -0.01104702316550528959, -159.4786160828277275, 1.513430353261248973 ) ) ;
#5774 = ORIENTED_EDGE ( 'NONE', *, *, #9875, .T. ) ;
#5775 = CARTESIAN_POINT ( 'NONE',  ( -0.4631675488762010962, -123.7427791793036391, 4.812436839529170562 ) ) ;
#5776 = CARTESIAN_POINT ( 'NONE',  ( 1.750805008852563294, -80.00120739911564272, 9.924274110580476815 ) ) ;
#5777 = CARTESIAN_POINT ( 'NONE',  ( -35.00000000000000711, -25.00000000000000711, -7.500000000000000000 ) ) ;
#5778 = ADVANCED_FACE ( 'NONE', ( #2509 ), #3325, .T. ) ;
#5779 = CARTESIAN_POINT ( 'NONE',  ( -35.00000000000000000, 25.00000000000000000, -7.500000000000000000 ) ) ;
#5780 = ORIENTED_EDGE ( 'NONE', *, *, #8985, .F. ) ;
#5781 = DIRECTION ( 'NONE',  ( -1.776356839400250465E-15, 0.000000000000000000, 1.000000000000000000 ) ) ;
#5782 = ORIENTED_EDGE ( 'NONE', *, *, #11052, .T. ) ;
#5783 = CYLINDRICAL_SURFACE ( 'NONE', #5039, 2.500000000000002220 ) ;
#5784 = B_SPLINE_CURVE_WITH_KNOTS ( 'NONE', 3,
 ( #989, #11707, #13785, #8420 ),
 .UNSPECIFIED., .F., .F.,
 ( 4, 4 ),
 ( 0.000000000000000000, 1.000000000000000000 ),
 .UNSPECIFIED. ) ;
#5785 = DIRECTION ( 'NONE',  ( 0.000000000000000000, 0.000000000000000000, -1.000000000000000000 ) ) ;
#5786 = FACE_OUTER_BOUND ( 'NONE', #4930, .T. ) ;
#5787 = AXIS2_PLACEMENT_3D ( 'NONE', #7215, #7280, #12762 ) ;
#5788 = CARTESIAN_POINT ( 'NONE',  ( -39.74871155318043492, 101.0697170996391492, -2.238193420436155989 ) ) ;
#5789 = LINE ( 'NONE', #8108, #8083 ) ;
#5790 = CARTESIAN_POINT ( 'NONE',  ( -15.29705854078139815, 64.91013567203349055, 30.59411708156277854 ) ) ;
#5791 = AXIS2_PLACEMENT_3D ( 'NONE', #11577, #3085, #11640 ) ;
#5792 = CARTESIAN_POINT ( 'NONE',  ( -15.29705854078139282, 55.48535772202409078, -9.797919878057798703E-17 ) ) ;
#5793 = CARTESIAN_POINT ( 'NONE',  ( 12.99553232110414847, -7.774801155466914970, -25.99106464220827917 ) ) ;
#5794 = VERTEX_POINT ( 'NONE', #764 ) ;
#5795 = CARTESIAN_POINT ( 'NONE',  ( -39.06230589874905945, 109.5835921350012825, 7.500000000000000000 ) ) ;
#5796 = ORIENTED_EDGE ( 'NONE', *, *, #13243, .F. ) ;
#5797 = CARTESIAN_POINT ( 'NONE',  ( 11.18807966363703876, -153.6493506493829102, -7.768796162325410926 ) ) ;
#5798 = VECTOR ( 'NONE', #8330, 999.9999999999998863 ) ;
#5799 = ORIENTED_EDGE ( 'NONE', *, *, #3702, .F. ) ;
#5800 = AXIS2_PLACEMENT_3D ( 'NONE', #10517, #5191, #4136 ) ;
#5801 = CARTESIAN_POINT ( 'NONE',  ( 8.385254915620295790, -31.79444290936001138, 1.085359338644428786E-15 ) ) ;
#5802 = ITEM_DEFINED_TRANSFORMATION ( 'NONE', 'NONE', #9990,  #8193 ) ;
#5803 = ORIENTED_EDGE ( 'NONE', *, *, #1814, .T. ) ;
#5804 = CARTESIAN_POINT ( 'NONE',  ( 12.99579180576516535, 35.80917582696438473, 1.535149190374665400E-15 ) ) ;
#5805 = CARTESIAN_POINT ( 'NONE',  ( 21.51985683731163945, -13.03114504999992995, 2.499999999999995559 ) ) ;
#5806 = LINE ( 'NONE', #13195, #4391 ) ;
#5807 = CARTESIAN_POINT ( 'NONE',  ( -15.29705854078139282, 19.67281349139177138, 30.59411708156277498 ) ) ;
#5808 = AXIS2_PLACEMENT_3D ( 'NONE', #10732, #170, #34 ) ;
#5809 = CARTESIAN_POINT ( 'NONE',  ( 15.29705854078139282, -38.76242177807012723, 3.746698755667522411E-15 ) ) ;
#5810 = CIRCLE ( 'NONE', #10926, 20.00000000000000000 ) ;
#5811 = ORIENTED_EDGE ( 'NONE', *, *, #13141, .F. ) ;
#5812 = DIRECTION ( 'NONE',  ( 0.000000000000000000, 0.000000000000000000, 1.000000000000000000 ) ) ;
#5813 = VECTOR ( 'NONE', #3436, 1000.000000000000000 ) ;
#5814 = ORIENTED_EDGE ( 'NONE', *, *, #5753, .F. ) ;
#5815 = ORIENTED_EDGE ( 'NONE', *, *, #7684, .F. ) ;
#5816 = CARTESIAN_POINT ( 'NONE',  ( 8.385254915620299343, -34.41905512736551032, 1.085359338644428786E-15 ) ) ;
#5817 = EDGE_CURVE ( 'NONE', #2958, #11894, #6229, .T. ) ;
#5818 = VECTOR ( 'NONE', #9575, 999.9999999999998863 ) ;
#5819 = FACE_OUTER_BOUND ( 'NONE', #700, .T. ) ;
#5820 = DIRECTION ( 'NONE',  ( 1.000000000000000000, 0.000000000000000000, 0.000000000000000000 ) ) ;
#5821 = DIRECTION ( 'NONE',  ( 0.9960067511297463483, -0.08927794634716619548, 0.000000000000000000 ) ) ;
#5822 = CARTESIAN_POINT ( 'NONE',  ( 8.296475850350821801, -93.99331153395371530, 1.275032287086958815 ) ) ;
#5823 = CARTESIAN_POINT ( 'NONE',  ( -10.69381717166375623, 16.13466892210585613, -2.653091794345379119E-15 ) ) ;
#5824 = EDGE_LOOP ( 'NONE', ( #1022, #4339, #6110, #2954 ) ) ;
#5825 = ORIENTED_EDGE ( 'NONE', *, *, #2497, .T. ) ;
#5826 = EDGE_LOOP ( 'NONE', ( #2689, #2148, #1901, #3223 ) ) ;
#5827 = CARTESIAN_POINT ( 'NONE',  ( -6.913174563124464989, -94.54126257933998545, -4.633799819412218746 ) ) ;
#5828 = AXIS2_PLACEMENT_3D ( 'NONE', #8579, #10479, #881 ) ;
#5829 = CIRCLE ( 'NONE', #13008, 15.29705854078139105 ) ;
#5830 = ORIENTED_EDGE ( 'NONE', *, *, #10628, .T. ) ;
#5831 = CARTESIAN_POINT ( 'NONE',  ( 35.00000000000000000, 4.286263797015736496E-15, 7.500000000000000000 ) ) ;
#5832 = CARTESIAN_POINT ( 'NONE',  ( 14.99223790936468603, -6.835163196276451636, 2.499999999999996891 ) ) ;
#5833 = ORIENTED_EDGE ( 'NONE', *, *, #9547, .T. ) ;
#5834 = CARTESIAN_POINT ( 'NONE',  ( 7.476762187090618461, -73.27151468276238688, 6.844715442818731788 ) ) ;
#5835 = ADVANCED_FACE ( 'NONE', ( #8191 ), #10626, .T. ) ;
#5836 = DIRECTION ( 'NONE',  ( -0.6001121574638170753, 0.7999158696163758409, 1.850470399461381402E-16 ) ) ;
#5837 = AXIS2_PLACEMENT_3D ( 'NONE', #12779, #12581, #8354 ) ;
#5838 = CARTESIAN_POINT ( 'NONE',  ( -4.114679947050897013, -133.0909090909224517, -0.08888163046369852716 ) ) ;
#5839 = CARTESIAN_POINT ( 'NONE',  ( 18.71826692230518674, -9.296782722394517862, 2.499999999999996447 ) ) ;
#5840 = EDGE_CURVE ( 'NONE', #7540, #4205, #1802, .T. ) ;
#5841 = CARTESIAN_POINT ( 'NONE',  ( -6.267146549262783140, -111.2727272727292700, 1.834821170859244344 ) ) ;
#5842 = EDGE_CURVE ( 'NONE', #8031, #13310, #7403, .T. ) ;
#5843 = CIRCLE ( 'NONE', #3132, 15.29705854078138927 ) ;
#5844 = DIRECTION ( 'NONE',  ( 0.000000000000000000, 0.000000000000000000, -1.000000000000000000 ) ) ;
#5845 = AXIS2_PLACEMENT_3D ( 'NONE', #606, #2627, #9010 ) ;
#5846 = DIRECTION ( 'NONE',  ( -0.9462100554738961389, -0.3235529800822216639, -1.445602896645893329E-16 ) ) ;
#5847 = EDGE_CURVE ( 'NONE', #3488, #8713, #12618, .T. ) ;
#5848 = CARTESIAN_POINT ( 'NONE',  ( -1.604942417060130136E-15, 57.37192529142945574, -1.013106070382630377E-16 ) ) ;
#5849 = ADVANCED_FACE ( 'NONE', ( #10362 ), #12474, .F. ) ;
#5850 = ORIENTED_EDGE ( 'NONE', *, *, #12901, .F. ) ;
#5851 = VERTEX_POINT ( 'NONE', #5030 ) ;
#5852 = ORIENTED_EDGE ( 'NONE', *, *, #1750, .T. ) ;
#5853 = CARTESIAN_POINT ( 'NONE',  ( -0.1852015970780942489, -159.9999997928953235, 1.488522644435750886 ) ) ;
#5854 = EDGE_LOOP ( 'NONE', ( #4536, #6445, #6552, #5891 ) ) ;
#5855 = CARTESIAN_POINT ( 'NONE',  ( 6.202303966384370426, -111.0571250337653879, -1.156479532967471302 ) ) ;
#5856 = CIRCLE ( 'NONE', #10105, 15.29705854078138749 ) ;
#5857 = CIRCLE ( 'NONE', #11228, 2.000000000000003109 ) ;
#5858 = DIRECTION ( 'NONE',  ( -1.000000000000000000, 0.000000000000000000, 0.000000000000000000 ) ) ;
#5859 = DIRECTION ( 'NONE',  ( 6.158143864569485777E-17, 2.736152283717910599E-16, -1.000000000000000000 ) ) ;
#5860 = VERTEX_POINT ( 'NONE', #5300 ) ;
#5861 = ORIENTED_EDGE ( 'NONE', *, *, #9043, .T. ) ;
#5862 = DIRECTION ( 'NONE',  ( 1.000000000000000000, 0.000000000000000000, 0.000000000000000000 ) ) ;
#5863 = ORIENTED_EDGE ( 'NONE', *, *, #3616, .T. ) ;
#5864 = CARTESIAN_POINT ( 'NONE',  ( 1.238865979958289509, -140.6626200957464334, 2.568243908262899389 ) ) ;
#5865 = EDGE_CURVE ( 'NONE', #7422, #5463, #6126, .T. ) ;
#5866 = CARTESIAN_POINT ( 'NONE',  ( 4.658064847839351152, 90.49194140877688142, -1.819915145876241036 ) ) ;
#5867 = DIRECTION ( 'NONE',  ( 0.8907235428302465730, 0.4545454545454549189, -0.000000000000000000 ) ) ;
#5868 = EDGE_CURVE ( 'NONE', #11234, #8040, #7664, .T. ) ;
#5869 = EDGE_CURVE ( 'NONE', #10278, #10788, #6553, .T. ) ;
#5870 = DIRECTION ( 'NONE',  ( -1.000000000000000000, 0.000000000000000000, 0.000000000000000000 ) ) ;
#5871 = CARTESIAN_POINT ( 'NONE',  ( -42.16244658108818300, 105.4500712252157797, 7.500000000000000000 ) ) ;
#5872 = LINE ( 'NONE', #10145, #2938 ) ;
#5873 = CARTESIAN_POINT ( 'NONE',  ( -8.385254915620294014, 62.45333659073424570, 16.77050983124057737 ) ) ;
#5874 = ADVANCED_FACE ( 'NONE', ( #833 ), #9581, .F. ) ;
#5875 = AXIS2_PLACEMENT_3D ( 'NONE', #7413, #10062, #2486 ) ;
#5876 = CARTESIAN_POINT ( 'NONE',  ( 8.385254915620295790, -6.144721277337255927, 1.035430912652129043E-15 ) ) ;
#5877 = VERTEX_POINT ( 'NONE', #9384 ) ;
#5878 = DIRECTION ( 'NONE',  ( -2.797435172181481150E-17, 1.000000000000000000, -1.765856845898762549E-18 ) ) ;
#5879 = ORIENTED_EDGE ( 'NONE', *, *, #11334, .F. ) ;
#5880 = CARTESIAN_POINT ( 'NONE',  ( -6.356408396254766835, -164.3636363616015217, -0.5463072361628438234 ) ) ;
#5881 = ORIENTED_EDGE ( 'NONE', *, *, #4625, .F. ) ;
#5882 = DIRECTION ( 'NONE',  ( 0.000000000000000000, 0.000000000000000000, 1.000000000000000000 ) ) ;
#5883 = CARTESIAN_POINT ( 'NONE',  ( -12.99579180576516002, 35.80917582696438473, -25.99158361153033070 ) ) ;
#5884 = DIRECTION ( 'NONE',  ( -1.000000000000000000, 0.000000000000000000, 0.000000000000000000 ) ) ;
#5885 = CARTESIAN_POINT ( 'NONE',  ( -35.00000000000000000, -20.00000000000000000, 7.500000000000000000 ) ) ;
#5886 = EDGE_CURVE ( 'NONE', #430, #10108, #7888, .T. ) ;
#5887 = DIRECTION ( 'NONE',  ( 1.000000000000000000, 0.000000000000000000, 0.000000000000000000 ) ) ;
#5888 = PRODUCT_DEFINITION_CONTEXT ( 'detailed design', #9879, 'design' ) ;
#5889 = CARTESIAN_POINT ( 'NONE',  ( 2.008006476061143353, -80.00378950643523979, 9.910921260988354575 ) ) ;
#5890 = ORIENTED_EDGE ( 'NONE', *, *, #6360, .F. ) ;
#5891 = ORIENTED_EDGE ( 'NONE', *, *, #8380, .T. ) ;
#5892 = CARTESIAN_POINT ( 'NONE',  ( 10.69346802281035202, -25.79937747632526879, -21.38693604562069339 ) ) ;
#5893 = ORIENTED_EDGE ( 'NONE', *, *, #13852, .T. ) ;
#5894 = CARTESIAN_POINT ( 'NONE',  ( 58.40844909094411719, 10.11407490371516360, -2.499999999999994671 ) ) ;
#5895 = CIRCLE ( 'NONE', #13746, 66.25000000000044054 ) ;
#5896 = DIRECTION ( 'NONE',  ( -0.000000000000000000, -0.000000000000000000, -1.000000000000000000 ) ) ;
#5897 = CARTESIAN_POINT ( 'NONE',  ( -8.043602924566211954, -72.64880124666912309, -6.161478634331895243 ) ) ;
#5898 = CARTESIAN_POINT ( 'NONE',  ( 38.81043356982896597, -18.35771219435081392, 2.499999999999995115 ) ) ;
#5899 = CARTESIAN_POINT ( 'NONE',  ( 7.733904924929606572, -95.38813776267139133, 2.765113012216059651 ) ) ;
#5900 = CARTESIAN_POINT ( 'NONE',  ( -8.385254915620294014, 50.40394642271930081, -16.77050983124059158 ) ) ;
#5901 = ORIENTED_EDGE ( 'NONE', *, *, #13592, .T. ) ;
#5902 = VECTOR ( 'NONE', #13699, 1000.000000000000000 ) ;
#5903 = EDGE_CURVE ( 'NONE', #4658, #7574, #10401, .T. ) ;
#5904 = ORIENTED_EDGE ( 'NONE', *, *, #8743, .T. ) ;
#5905 = CARTESIAN_POINT ( 'NONE',  ( 9.456627357064096628, -73.18181818181959386, 3.908318357316015401 ) ) ;
#5906 = ORIENTED_EDGE ( 'NONE', *, *, #352, .T. ) ;
#5907 = DIRECTION ( 'NONE',  ( 6.158143864569485777E-17, 2.736152283717910599E-16, -1.000000000000000000 ) ) ;
#5908 = SURFACE_SIDE_STYLE ('',( #10249 ) ) ;
#5909 = DIRECTION ( 'NONE',  ( -1.601283208593975514E-16, 1.000000000000000000, 0.000000000000000000 ) ) ;
#5910 = CARTESIAN_POINT ( 'NONE',  ( -12.99553232110414491, -17.19957910547634228, -3.161261631924336761E-15 ) ) ;
#5911 = CARTESIAN_POINT ( 'NONE',  ( -3.628753873973424415, -79.03030303036898374, -9.983370075638070773 ) ) ;
#5912 = CARTESIAN_POINT ( 'NONE',  ( 0.000000000000000000, -20.00000000000000000, 0.000000000000000000 ) ) ;
#5913 = B_SPLINE_CURVE_WITH_KNOTS ( 'NONE', 3,
 ( #6762, #1433, #2562, #5710 ),
 .UNSPECIFIED., .F., .F.,
 ( 4, 4 ),
 ( 0.000000000000000000, 1.000000000000000000 ),
 .UNSPECIFIED. ) ;
#5914 = DIRECTION ( 'NONE',  ( 1.000000000000000000, 0.000000000000000000, 0.000000000000000000 ) ) ;
#5915 = DIRECTION ( 'NONE',  ( 1.000000000000000000, 1.156482317317871133E-15, 0.000000000000000000 ) ) ;
#5916 = EDGE_LOOP ( 'NONE', ( #12639, #5770, #10966, #4192 ) ) ;
#5917 = ORIENTED_EDGE ( 'NONE', *, *, #13339, .T. ) ;
#5918 = ORIENTED_EDGE ( 'NONE', *, *, #10219, .F. ) ;
#5919 = ORIENTED_EDGE ( 'NONE', *, *, #8489, .F. ) ;
#5920 = AXIS2_PLACEMENT_3D ( 'NONE', #7249, #11600, #11534 ) ;
#5921 = ADVANCED_FACE ( 'NONE', ( #12546 ), #8390, .T. ) ;
#5922 = CARTESIAN_POINT ( 'NONE',  ( 1.479030741744671973, -121.1096557515223680, 4.854982109747082220 ) ) ;
#5923 = FACE_OUTER_BOUND ( 'NONE', #11346, .T. ) ;
#5924 = EDGE_CURVE ( 'NONE', #42, #8113, #8346, .T. ) ;
#5925 = CARTESIAN_POINT ( 'NONE',  ( 45.47624229149391084, 15.54906262289183871, -2.499999999999994671 ) ) ;
#5926 = CIRCLE ( 'NONE', #6147, 15.29705854078138572 ) ;
#5927 = DIRECTION ( 'NONE',  ( -6.158143864569485777E-17, -2.736152283717910599E-16, 1.000000000000000000 ) ) ;
#5928 = DIRECTION ( 'NONE',  ( -2.797435172181481150E-17, 1.000000000000000000, -1.765856845898762549E-18 ) ) ;
#5929 = EDGE_CURVE ( 'NONE', #4671, #12589, #7446, .T. ) ;
#5930 = ORIENTED_EDGE ( 'NONE', *, *, #4702, .T. ) ;
#5931 = DIRECTION ( 'NONE',  ( 0.000000000000000000, 0.000000000000000000, 1.000000000000000000 ) ) ;
#5932 = CARTESIAN_POINT ( 'NONE',  ( 3.705099044711014589, -132.0105060180018768, -0.8975303730290892235 ) ) ;
#5933 = LINE ( 'NONE', #8033, #7808 ) ;
#5934 = CARTESIAN_POINT ( 'NONE',  ( 15.29705854078139282, -38.76242177807012723, 1.940132561565339224E-15 ) ) ;
#5935 = VECTOR ( 'NONE', #9337, 1000.000000000000000 ) ;
#5936 = DIRECTION ( 'NONE',  ( 0.000000000000000000, 1.000000000000000000, 0.000000000000000000 ) ) ;
#5937 = CARTESIAN_POINT ( 'NONE',  ( -40.34010237645985342, 100.7894366958197878, -1.747896926826553843 ) ) ;
#5938 = CARTESIAN_POINT ( 'NONE',  ( 62.16766351966359849, -73.17985663200910551, -2.500000000000000000 ) ) ;
#5939 = CIRCLE ( 'NONE', #4127, 15.00000000000000000 ) ;
#5940 = EDGE_CURVE ( 'NONE', #8621, #10317, #11684, .T. ) ;
#5941 = VERTEX_POINT ( 'NONE', #8658 ) ;
#5942 = ORIENTED_EDGE ( 'NONE', *, *, #5265, .F. ) ;
#5943 = EDGE_CURVE ( 'NONE', #13056, #12718, #1862, .T. ) ;
#5944 = CARTESIAN_POINT ( 'NONE',  ( -0.003226301100687127901, -100.2727272727200756, -4.613888802083975449 ) ) ;
#5945 = AXIS2_PLACEMENT_3D ( 'NONE', #6016, #4958, #758 ) ;
#5946 = ORIENTED_EDGE ( 'NONE', *, *, #13247, .T. ) ;
#5947 = AXIS2_PLACEMENT_3D ( 'NONE', #13021, #252, #13098 ) ;
#5948 = ADVANCED_FACE ( 'NONE', ( #3261 ), #7536, .T. ) ;
#5949 = ORIENTED_EDGE ( 'NONE', *, *, #13247, .F. ) ;
#5950 = CARTESIAN_POINT ( 'NONE',  ( -4.974937185533102380, 90.00000000000000000, -0.5000000000000000000 ) ) ;
#5951 = EDGE_CURVE ( 'NONE', #11359, #4067, #11565, .T. ) ;
#5952 = DIRECTION ( 'NONE',  ( -0.000000000000000000, -0.000000000000000000, 1.000000000000000000 ) ) ;
#5953 = CARTESIAN_POINT ( 'NONE',  ( -10.12341346681890819, -72.18181818172617170, -6.554034102534079587 ) ) ;
#5954 = AXIS2_PLACEMENT_3D ( 'NONE', #2560, #11946, #3521 ) ;
#5955 = DIRECTION ( 'NONE',  ( 1.000000000000000000, 0.000000000000000000, 0.000000000000000000 ) ) ;
#5956 = CARTESIAN_POINT ( 'NONE',  ( -2.403405165857241954E-13, -159.9999999999998010, -2.442165393523598738E-13 ) ) ;
#5957 = CIRCLE ( 'NONE', #5053, 2.000000000000003109 ) ;
#5958 = ORIENTED_EDGE ( 'NONE', *, *, #6216, .T. ) ;
#5959 = ORIENTED_EDGE ( 'NONE', *, *, #10645, .T. ) ;
#5960 = ADVANCED_FACE ( 'NONE', ( #3462 ), #4379, .T. ) ;
#5961 = CARTESIAN_POINT ( 'NONE',  ( -3.122627689365423453, -81.55733635889028221, 9.361082846595628837 ) ) ;
#5962 = AXIS2_PLACEMENT_3D ( 'NONE', #8100, #667, #3593 ) ;
#5963 = EDGE_CURVE ( 'NONE', #420, #6463, #2281, .T. ) ;
#5964 = ORIENTED_EDGE ( 'NONE', *, *, #4437, .F. ) ;
#5965 = ORIENTED_EDGE ( 'NONE', *, *, #3281, .T. ) ;
#5966 = DIRECTION ( 'NONE',  ( 0.000000000000000000, 1.000000000000000000, 0.000000000000000000 ) ) ;
#5967 = AXIS2_PLACEMENT_3D ( 'NONE', #8428, #11517, #4997 ) ;
#5968 = DIRECTION ( 'NONE',  ( 1.000000000000000000, 0.000000000000000000, 0.000000000000000000 ) ) ;
#5969 = CARTESIAN_POINT ( 'NONE',  ( 19.84413750617685324, 26.75684992538831963, -2.573597559463546069 ) ) ;
#5970 = DIRECTION ( 'NONE',  ( -6.158143864569485777E-17, -2.736152283717910599E-16, 1.000000000000000000 ) ) ;
#5971 = CARTESIAN_POINT ( 'NONE',  ( 4.606570477487116122, -99.66561582491799243, 6.166945419414991747 ) ) ;
#5972 = CARTESIAN_POINT ( 'NONE',  ( -10.69346802281035025, 49.59884612375012125, -2.736290265663450252E-15 ) ) ;
#5973 = CIRCLE ( 'NONE', #6398, 50.00000000000001421 ) ;
#5974 = ORIENTED_EDGE ( 'NONE', *, *, #6362, .T. ) ;
#5975 = ORIENTED_EDGE ( 'NONE', *, *, #3614, .T. ) ;
#5976 = ORIENTED_EDGE ( 'NONE', *, *, #3693, .T. ) ;
#5977 = CARTESIAN_POINT ( 'NONE',  ( 30.92745768374916082, -20.74715399464528787, -2.500000000000005329 ) ) ;
#5978 = ORIENTED_EDGE ( 'NONE', *, *, #13566, .F. ) ;
#5979 = CARTESIAN_POINT ( 'NONE',  ( -15.29705854078139460, -27.45107625865536605, -1.776400035956490916E-15 ) ) ;
#5980 = VECTOR ( 'NONE', #11119, 1000.000000000000000 ) ;
#5981 = CARTESIAN_POINT ( 'NONE',  ( -24.37649275748776390, -100.0000000000000000, 7.500000000000000000 ) ) ;
#5982 = ORIENTED_EDGE ( 'NONE', *, *, #10986, .F. ) ;
#5983 = CARTESIAN_POINT ( 'NONE',  ( 8.558795037935681194, -72.03745727283919109, 5.439008144249546817 ) ) ;
#5984 = CARTESIAN_POINT ( 'NONE',  ( -5.655105406264300250, -85.78354978356081517, 8.815184813460382074 ) ) ;
#5985 = FACE_OUTER_BOUND ( 'NONE', #938, .T. ) ;
#5986 = DIRECTION ( 'NONE',  ( -6.158143864569485777E-17, -2.736152283717910599E-16, 1.000000000000000000 ) ) ;
#5987 = CARTESIAN_POINT ( 'NONE',  ( -5.770059030975961178, -111.2727272727253904, 3.008649887263203926 ) ) ;
#5988 = DIRECTION ( 'NONE',  ( -1.000000000000000000, 0.000000000000000000, 0.000000000000000000 ) ) ;
#5989 = CARTESIAN_POINT ( 'NONE',  ( 8.385254915620288685, 34.17900274070598243, 9.688596779957292534E-16 ) ) ;
#5990 = ORIENTED_EDGE ( 'NONE', *, *, #8238, .F. ) ;
#5991 = VERTEX_POINT ( 'NONE', #11815 ) ;
#5992 = TOROIDAL_SURFACE ( 'NONE', #7087, 77.99999999999997158, 2.000000000000000000 ) ;
#5993 = ORIENTED_EDGE ( 'NONE', *, *, #2967, .T. ) ;
#5994 = CARTESIAN_POINT ( 'NONE',  ( 1.403442481258843078, -154.8168939350541393, 0.8939811563333199818 ) ) ;
#5995 = ORIENTED_EDGE ( 'NONE', *, *, #1816, .F. ) ;
#5996 = CARTESIAN_POINT ( 'NONE',  ( 3.916815862944407645, -105.5671819316534936, -5.801851910426949921 ) ) ;
#5997 = CARTESIAN_POINT ( 'NONE',  ( -19.18070798040252356, 20.00000000000000000, -4.000000000000000000 ) ) ;
#5998 = DIRECTION ( 'NONE',  ( -0.000000000000000000, -0.000000000000000000, -1.000000000000000000 ) ) ;
#5999 = CARTESIAN_POINT ( 'NONE',  ( 39.08445607832919677, 20.74481184150345214, -2.499999999999992895 ) ) ;
#6000 = ORIENTED_EDGE ( 'NONE', *, *, #3097, .F. ) ;
#6001 = CARTESIAN_POINT ( 'NONE',  ( -2.237684797877293663E-15, 79.99058638175036151, -1.412519245696701158E-16 ) ) ;
#6002 = CARTESIAN_POINT ( 'NONE',  ( 2.144143433502907037, -126.4672479063739559, -3.929051445287345512 ) ) ;
#6003 = CARTESIAN_POINT ( 'NONE',  ( 22.84091969677297485, -17.29701610032388359, -2.500000000000004441 ) ) ;
#6004 = CARTESIAN_POINT ( 'NONE',  ( 34.99999999999958789, 1.091249486606660213E-13, 2.500000000000000000 ) ) ;
#6005 = EDGE_CURVE ( 'NONE', #5594, #2949, #11490, .T. ) ;
#6006 = DIRECTION ( 'NONE',  ( 1.000000000000000000, 0.000000000000000000, 0.000000000000000000 ) ) ;
#6007 = CARTESIAN_POINT ( 'NONE',  ( 76.84607712649204814, -99.92541302764922762, 2.500000000000000000 ) ) ;
#6008 = LINE ( 'NONE', #4947, #11224 ) ;
#6009 = FACE_OUTER_BOUND ( 'NONE', #11133, .T. ) ;
#6010 = ORIENTED_EDGE ( 'NONE', *, *, #4983, .F. ) ;
#6011 = ORIENTED_EDGE ( 'NONE', *, *, #12123, .F. ) ;
#6012 = CARTESIAN_POINT ( 'NONE',  ( 12.97432671025186224, -68.90909090921057611, 1.142286363980197006 ) ) ;
#6013 = ORIENTED_EDGE ( 'NONE', *, *, #2999, .T. ) ;
#6014 = EDGE_LOOP ( 'NONE', ( #5879, #8991, #5314 ) ) ;
#6015 = CARTESIAN_POINT ( 'NONE',  ( 17.38503225228318883, -6.421675190136373779, -2.500000000000002665 ) ) ;
#6016 = CARTESIAN_POINT ( 'NONE',  ( 39.06230589874905235, 109.5835921350012683, 7.500000000000000000 ) ) ;
#6017 = CARTESIAN_POINT ( 'NONE',  ( 3.042673274263369976, -100.2727272727297105, 12.70187379131525418 ) ) ;
#6018 = CIRCLE ( 'NONE', #8470, 22.00000000000000355 ) ;
#6019 = EDGE_CURVE ( 'NONE', #9459, #4575, #1367, .T. ) ;
#6020 = CARTESIAN_POINT ( 'NONE',  ( 10.69381717166375267, -21.56444287793185310, 21.38763434332751601 ) ) ;
#6021 = ADVANCED_FACE ( 'NONE', ( #5361 ), #9854, .T. ) ;
#6022 = DIRECTION ( 'NONE',  ( 0.000000000000000000, -1.000000000000000000, 0.000000000000000000 ) ) ;
#6023 = CARTESIAN_POINT ( 'NONE',  ( -4.961407659643952250, 90.00000000000001421, 0.6346170828971220423 ) ) ;
#6024 = ADVANCED_FACE ( 'NONE', ( #7673 ), #12959, .T. ) ;
#6025 = ORIENTED_EDGE ( 'NONE', *, *, #11862, .T. ) ;
#6026 = EDGE_CURVE ( 'NONE', #3686, #2454, #13550, .T. ) ;
#6027 = CIRCLE ( 'NONE', #13886, 15.29705854078139460 ) ;
#6028 = CIRCLE ( 'NONE', #7139, 25.50000000002549783 ) ;
#6029 = ORIENTED_EDGE ( 'NONE', *, *, #8487, .T. ) ;
#6030 = VERTEX_POINT ( 'NONE', #4442 ) ;
#6031 = CARTESIAN_POINT ( 'NONE',  ( -8.385254915620290461, -12.94488700934118341, -16.77050983124058803 ) ) ;
#6032 = ADVANCED_FACE ( 'NONE', ( #11751 ), #10891, .F. ) ;
#6033 = CARTESIAN_POINT ( 'NONE',  ( 0.000000000000000000, 0.000000000000000000, 0.000000000000000000 ) ) ;
#6034 = CARTESIAN_POINT ( 'NONE',  ( -35.00000000000000000, -35.00000000000000000, 4.000000000000000000 ) ) ;
#6035 = CARTESIAN_POINT ( 'NONE',  ( 28.15981099771517648, -27.70535714287384721, 7.500000000000000000 ) ) ;
#6036 = CARTESIAN_POINT ( 'NONE',  ( 4.498378629186895239, -85.01274099036943710, -8.404829403884384931 ) ) ;
#6037 = VECTOR ( 'NONE', #6333, 1000.000000000000114 ) ;
#6038 = CYLINDRICAL_SURFACE ( 'NONE', #10701, 5.000000000000000000 ) ;
#6039 = EDGE_CURVE ( 'NONE', #5217, #3291, #8129, .T. ) ;
#6040 = ORIENTED_EDGE ( 'NONE', *, *, #4821, .F. ) ;
#6041 = DIRECTION ( 'NONE',  ( -6.158143864569485777E-17, -2.736152283717910599E-16, 1.000000000000000000 ) ) ;
#6042 = AXIS2_PLACEMENT_3D ( 'NONE', #4748, #9023, #10964 ) ;
#6043 = ORIENTED_EDGE ( 'NONE', *, *, #12796, .F. ) ;
#6044 = DIRECTION ( 'NONE',  ( -1.224646799147353207E-16, 1.000000000000000000, -0.000000000000000000 ) ) ;
#6045 = CIRCLE ( 'NONE', #8716, 22.99999999999999645 ) ;
#6046 = DIRECTION ( 'NONE',  ( -0.9960067511297463483, 0.08927794634716618161, -4.818676322152979407E-17 ) ) ;
#6047 = ORIENTED_EDGE ( 'NONE', *, *, #874, .T. ) ;
#6048 = CARTESIAN_POINT ( 'NONE',  ( 4.711442140758930641, -75.83792211546017370, 8.965827202672375762 ) ) ;
#6049 =( NAMED_UNIT ( * ) SI_UNIT ( $, .STERADIAN. ) SOLID_ANGLE_UNIT ( ) );
#6050 = CARTESIAN_POINT ( 'NONE',  ( 10.69381717166375445, 44.40900277213413716, 2.619229793989003951E-15 ) ) ;
#6051 = DIRECTION ( 'NONE',  ( -0.000000000000000000, -0.000000000000000000, -1.000000000000000000 ) ) ;
#6052 = DIRECTION ( 'NONE',  ( 2.797435172181480534E-17, -1.000000000000000000, 1.765856845898762164E-18 ) ) ;
#6053 = DIRECTION ( 'NONE',  ( 0.000000000000000000, 0.000000000000000000, 1.000000000000000000 ) ) ;
#6054 = DIRECTION ( 'NONE',  ( 1.000000000000000000, -3.851859888774468203E-30, 1.387778780781445676E-15 ) ) ;
#6055 = DIRECTION ( 'NONE',  ( -0.9960067511297463483, 0.08927794634716618161, -4.818676322152979407E-17 ) ) ;
#6056 = VERTEX_POINT ( 'NONE', #9719 ) ;
#6057 = ADVANCED_FACE ( 'NONE', ( #10822 ), #128, .T. ) ;
#6058 = CIRCLE ( 'NONE', #7605, 2.500000000000002220 ) ;
#6059 = AXIS2_PLACEMENT_3D ( 'NONE', #7692, #11974, #5595 ) ;
#6060 = ORIENTED_EDGE ( 'NONE', *, *, #9198, .F. ) ;
#6061 = ORIENTED_EDGE ( 'NONE', *, *, #12991, .T. ) ;
#6062 = CARTESIAN_POINT ( 'NONE',  ( 5.365917630196002541, -107.8841580301423448, -3.999906080763434346 ) ) ;
#6063 = DIRECTION ( 'NONE',  ( 0.000000000000000000, 1.000000000000000000, 0.000000000000000000 ) ) ;
#6064 = CIRCLE ( 'NONE', #2014, 5.000000000000005329 ) ;
#6065 = FACE_OUTER_BOUND ( 'NONE', #296, .T. ) ;
#6066 = CARTESIAN_POINT ( 'NONE',  ( -2.517691654963332357E-15, 90.00000000000000000, -1.589271161308885878E-16 ) ) ;
#6067 = AXIS2_PLACEMENT_3D ( 'NONE', #8101, #2834, #13599 ) ;
#6068 = DIRECTION ( 'NONE',  ( -6.158143864569485777E-17, -2.736152283717910599E-16, 1.000000000000000000 ) ) ;
#6069 = DIRECTION ( 'NONE',  ( 0.000000000000000000, 0.000000000000000000, 1.000000000000000000 ) ) ;
#6070 = CARTESIAN_POINT ( 'NONE',  ( -39.99999999999999289, 100.0000000000000000, 0.5000000000000000000 ) ) ;
#6071 = FACE_OUTER_BOUND ( 'NONE', #7369, .T. ) ;
#6072 = CARTESIAN_POINT ( 'NONE',  ( -35.00000000000000000, -4.286263797015736496E-15, -4.000000000000000000 ) ) ;
#6073 = AXIS2_PLACEMENT_3D ( 'NONE', #2218, #3135, #1181 ) ;
#6074 = VECTOR ( 'NONE', #11838, 1000.000000000000000 ) ;
#6075 = VERTEX_POINT ( 'NONE', #1239 ) ;
#6076 = VECTOR ( 'NONE', #5812, 1000.000000000000000 ) ;
#6077 = CARTESIAN_POINT ( 'NONE',  ( 8.385254915620288685, 71.87811454074363837, 9.022884433393296612E-16 ) ) ;
#6078 = CARTESIAN_POINT ( 'NONE',  ( 34.99999999999958789, 1.063887963769481123E-13, 12.50000000000000000 ) ) ;
#6079 = EDGE_CURVE ( 'NONE', #4734, #10317, #12626, .T. ) ;
#6080 = ORIENTED_EDGE ( 'NONE', *, *, #3373, .F. ) ;
#6081 = DIRECTION ( 'NONE',  ( 1.000000000000000000, 0.000000000000000000, 0.000000000000000000 ) ) ;
#6082 = CARTESIAN_POINT ( 'NONE',  ( 12.99553232110413781, 58.19864449459907974, 0.000000000000000000 ) ) ;
#6083 = DIRECTION ( 'NONE',  ( -1.000000000000000000, 0.000000000000000000, 0.000000000000000000 ) ) ;
#6084 = ITEM_DEFINED_TRANSFORMATION ( 'NONE', 'NONE', #3473,  #8193 ) ;
#6085 = CARTESIAN_POINT ( 'NONE',  ( -4.481549108000151271, -153.6493506493174550, 1.751282401330790162 ) ) ;
#6086 = AXIS2_PLACEMENT_3D ( 'NONE', #6900, #5867, #2707 ) ;
#6087 = B_SPLINE_CURVE_WITH_KNOTS ( 'NONE', 3,
 ( #2443, #10099, #12208, #10993 ),
 .UNSPECIFIED., .F., .F.,
 ( 4, 4 ),
 ( 0.000000000000000000, 1.000000000000000000 ),
 .UNSPECIFIED. ) ;
#6088 = VECTOR ( 'NONE', #6218, 999.9999999999998863 ) ;
#6089 = DIRECTION ( 'NONE',  ( 1.000000000000000000, 0.000000000000000000, 0.000000000000000000 ) ) ;
#6090 = CARTESIAN_POINT ( 'NONE',  ( 48.99302833075611119, 12.47878836808090064, -2.499999999999994671 ) ) ;
#6091 = CARTESIAN_POINT ( 'NONE',  ( -32.50000000000000000, -3.980102097228898626E-15, 7.500000000000000000 ) ) ;
#6092 = B_SPLINE_CURVE_WITH_KNOTS ( 'NONE', 3,
 ( #6928, #8058, #10991, #11069 ),
 .UNSPECIFIED., .F., .F.,
 ( 4, 4 ),
 ( 0.000000000000000000, 1.000000000000000000 ),
 .UNSPECIFIED. ) ;
#6093 = CARTESIAN_POINT ( 'NONE',  ( 12.97449437267217043, -39.59556244224027211, 25.94898874534434796 ) ) ;
#6094 = ORIENTED_EDGE ( 'NONE', *, *, #6602, .F. ) ;
#6095 = ORIENTED_EDGE ( 'NONE', *, *, #9620, .F. ) ;
#6096 = AXIS2_PLACEMENT_3D ( 'NONE', #12530, #12732, #8312 ) ;
#6097 = EDGE_CURVE ( 'NONE', #1633, #2083, #9472, .T. ) ;
#6098 = EDGE_CURVE ( 'NONE', #7969, #6913, #968, .T. ) ;
#6099 = VERTEX_POINT ( 'NONE', #2493 ) ;
#6100 = EDGE_CURVE ( 'NONE', #2744, #10763, #3872, .T. ) ;
#6101 =( NAMED_UNIT ( * ) SI_UNIT ( $, .STERADIAN. ) SOLID_ANGLE_UNIT ( ) );
#6102 = CARTESIAN_POINT ( 'NONE',  ( -24.37649275748776390, -100.0000000000000000, 7.500000000000000000 ) ) ;
#6103 = EDGE_CURVE ( 'NONE', #11376, #7898, #11703, .T. ) ;
#6104 = CARTESIAN_POINT ( 'NONE',  ( 8.385254915620295790, 31.55439052270045508, 9.996449125125102610E-16 ) ) ;
#6105 = DIRECTION ( 'NONE',  ( -6.158143864569485777E-17, -2.736152283717910599E-16, 1.000000000000000000 ) ) ;
#6106 = AXIS2_PLACEMENT_3D ( 'NONE', #2651, #9166, #1009 ) ;
#6107 = SPHERICAL_SURFACE ( 'NONE', #1471, 5.000000000000000000 ) ;
#6108 = LINE ( 'NONE', #775, #11701 ) ;
#6109 = CARTESIAN_POINT ( 'NONE',  ( -2.517691654963332357E-15, 90.00000000000000000, -1.589271161308885878E-16 ) ) ;
#6110 = ORIENTED_EDGE ( 'NONE', *, *, #5070, .F. ) ;
#6111 = ADVANCED_FACE ( 'NONE', ( #11040 ), #413, .T. ) ;
#6112 = EDGE_CURVE ( 'NONE', #11046, #11396, #1526, .T. ) ;
#6113 = ORIENTED_EDGE ( 'NONE', *, *, #7100, .T. ) ;
#6114 = CARTESIAN_POINT ( 'NONE',  ( -2.482729886976823952, 90.00000000000001421, -4.353114590951097540 ) ) ;
#6115 = ORIENTED_EDGE ( 'NONE', *, *, #13626, .T. ) ;
#6116 = CARTESIAN_POINT ( 'NONE',  ( 11.81226048336477064, -40.00941361824966691, 1.498154114293980678E-15 ) ) ;
#6117 = ORIENTED_EDGE ( 'NONE', *, *, #11756, .T. ) ;
#6118 = EDGE_CURVE ( 'NONE', #13042, #3901, #12100, .T. ) ;
#6119 = CARTESIAN_POINT ( 'NONE',  ( 16.85679715600144135, -10.85606698379832125, 2.499999999999996003 ) ) ;
#6120 = ADVANCED_FACE ( 'NONE', ( #6771 ), #13259, .T. ) ;
#6121 = DIRECTION ( 'NONE',  ( -6.158143864569485777E-17, -2.736152283717910599E-16, 1.000000000000000000 ) ) ;
#6122 = CARTESIAN_POINT ( 'NONE',  ( 25.00000000000000355, 120.0000000000000284, -0.5000000000000000000 ) ) ;
#6123 = DIRECTION ( 'NONE',  ( -1.000000000000000000, 0.000000000000000000, 0.000000000000000000 ) ) ;
#6124 = CIRCLE ( 'NONE', #13547, 17.49999999999999645 ) ;
#6125 = CARTESIAN_POINT ( 'NONE',  ( -2.992550472303094455, -137.9200387812562667, 0.9708280758990516235 ) ) ;
#6126 = CIRCLE ( 'NONE', #9916, 22.99999999999999645 ) ;
#6127 = DIRECTION ( 'NONE',  ( -2.797435172181479917E-17, 1.000000000000000000, -1.765856845898779112E-18 ) ) ;
#6128 = ORIENTED_EDGE ( 'NONE', *, *, #8733, .F. ) ;
#6129 = VERTEX_POINT ( 'NONE', #5792 ) ;
#6130 = VERTEX_POINT ( 'NONE', #5536 ) ;
#6131 = AXIS2_PLACEMENT_3D ( 'NONE', #2036, #10587, #8480 ) ;
#6132 = EDGE_CURVE ( 'NONE', #3347, #5217, #12844, .T. ) ;
#6133 = CARTESIAN_POINT ( 'NONE',  ( 1.718945942447514764E-16, -6.144721277337255927, 1.085069813372578838E-17 ) ) ;
#6134 = AXIS2_PLACEMENT_3D ( 'NONE', #1397, #8905, #157 ) ;
#6135 = CARTESIAN_POINT ( 'NONE',  ( 40.81228451836345528, 100.6358150620708329, 0.5000000000000000000 ) ) ;
#6136 = CARTESIAN_POINT ( 'NONE',  ( -5.865056423939742913, -109.1014366316559290, 2.931634662963101157 ) ) ;
#6137 = EDGE_CURVE ( 'NONE', #430, #1472, #8562, .T. ) ;
#6138 = DIRECTION ( 'NONE',  ( 0.6000000000000001998, -0.7999999999999999334, 0.000000000000000000 ) ) ;
#6139 = FACE_OUTER_BOUND ( 'NONE', #9682, .T. ) ;
#6140 = DIRECTION ( 'NONE',  ( 0.4545454545454531425, 0.8907235428302472391, 0.000000000000000000 ) ) ;
#6141 = DIRECTION ( 'NONE',  ( -0.6001121574638169642, 0.7999158696163758409, 1.927470528861191270E-16 ) ) ;
#6142 = CIRCLE ( 'NONE', #10816, 18.74900000001875355 ) ;
#6143 = DIRECTION ( 'NONE',  ( 0.000000000000000000, 0.000000000000000000, 1.000000000000000000 ) ) ;
#6144 = CARTESIAN_POINT ( 'NONE',  ( 15.29705854078138927, 29.09759144140119957, 3.746698755667522411E-15 ) ) ;
#6145 = CIRCLE ( 'NONE', #558, 24.99999999999998934 ) ;
#6146 = CARTESIAN_POINT ( 'NONE',  ( 38.81043356982896597, -18.35771219435081392, -2.500000000000004441 ) ) ;
#6147 = AXIS2_PLACEMENT_3D ( 'NONE', #10830, #10899, #7752 ) ;
#6148 = ORIENTED_EDGE ( 'NONE', *, *, #99, .F. ) ;
#6149 = CARTESIAN_POINT ( 'NONE',  ( 15.29705854078140348, -29.33764382806072746, 1.923489752901241150E-15 ) ) ;
#6150 = CARTESIAN_POINT ( 'NONE',  ( -4.242345193642410806, -72.18181818157590612, -0.3889582016414882548 ) ) ;
#6151 = VERTEX_POINT ( 'NONE', #1206 ) ;
#6152 = LINE ( 'NONE', #5090, #1689 ) ;
#6153 = ORIENTED_EDGE ( 'NONE', *, *, #448, .F. ) ;
#6154 = VECTOR ( 'NONE', #2350, 1000.000000000000000 ) ;
#6155 = CARTESIAN_POINT ( 'NONE',  ( 43.63403238902020576, 20.33700654369049587, -2.499999999999992895 ) ) ;
#6156 = CYLINDRICAL_SURFACE ( 'NONE', #7476, 22.00000000000000000 ) ;
#6157 = CARTESIAN_POINT ( 'NONE',  ( 14.41066181492265130, -21.94006687227777519, 6.364279405527199174 ) ) ;
#6158 = CARTESIAN_POINT ( 'NONE',  ( -3.784192700541099352, -60.99999999999985789, -1.982393907671068822 ) ) ;
#6159 = DIRECTION ( 'NONE',  ( 1.000000000000000000, 0.000000000000000000, -0.000000000000000000 ) ) ;
#6160 = CARTESIAN_POINT ( 'NONE',  ( -42.16244658108818300, 105.4500712252157797, 2.499999999999999556 ) ) ;
#6161 = DIRECTION ( 'NONE',  ( 0.000000000000000000, -1.000000000000000000, 0.000000000000000000 ) ) ;
#6162 = AXIS2_PLACEMENT_3D ( 'NONE', #10011, #5512, #10768 ) ;
#6163 = CARTESIAN_POINT ( 'NONE',  ( 42.16244658108818300, 105.4500712252157655, 2.499999999999999556 ) ) ;
#6164 = VECTOR ( 'NONE', #2273, 1000.000000000000000 ) ;
#6165 = ORIENTED_EDGE ( 'NONE', *, *, #2363, .T. ) ;
#6166 = AXIS2_PLACEMENT_3D ( 'NONE', #10411, #4020, #5210 ) ;
#6167 = CARTESIAN_POINT ( 'NONE',  ( -7.205014192377404036, -85.42868670995821390, 6.118711583836721424 ) ) ;
#6168 = ORIENTED_EDGE ( 'NONE', *, *, #3163, .F. ) ;
#6169 = DIRECTION ( 'NONE',  ( -1.000000000000000000, 0.000000000000000000, 0.000000000000000000 ) ) ;
#6170 = AXIS2_PLACEMENT_3D ( 'NONE', #6466, #94, #2460 ) ;
#6171 = DIRECTION ( 'NONE',  ( 0.4226182617407014397, -0.9063077870366489375, -0.000000000000000000 ) ) ;
#6172 = DIRECTION ( 'NONE',  ( 0.000000000000000000, 0.000000000000000000, 1.000000000000000000 ) ) ;
#6173 = AXIS2_PLACEMENT_3D ( 'NONE', #13884, #959, #3186 ) ;
#6174 = DIRECTION ( 'NONE',  ( 0.000000000000000000, -1.000000000000000000, 0.000000000000000000 ) ) ;
#6175 = CARTESIAN_POINT ( 'NONE',  ( 0.7725026565705566117, -151.5832121717045311, 1.650885043546370001 ) ) ;
#6176 = ADVANCED_FACE ( 'NONE', ( #3230 ), #12403, .T. ) ;
#6177 = DIRECTION ( 'NONE',  ( -1.000000000000000000, 0.000000000000000000, -0.000000000000000000 ) ) ;
#6178 = EDGE_CURVE ( 'NONE', #10530, #4194, #4534, .T. ) ;
#6179 = ORIENTED_EDGE ( 'NONE', *, *, #4650, .T. ) ;
#6180 = ORIENTED_EDGE ( 'NONE', *, *, #11890, .F. ) ;
#6181 = VECTOR ( 'NONE', #8026, 1000.000000000000000 ) ;
#6182 = FACE_OUTER_BOUND ( 'NONE', #2585, .T. ) ;
#6183 = AXIS2_PLACEMENT_3D ( 'NONE', #13306, #3658, #10122 ) ;
#6184 = VERTEX_POINT ( 'NONE', #8696 ) ;
#6185 = CARTESIAN_POINT ( 'NONE',  ( 30.45476892764376231, 18.18971895053902443, -2.499999999999993783 ) ) ;
#6186 = EDGE_LOOP ( 'NONE', ( #10280, #685, #11788, #9803 ) ) ;
#6187 = EDGE_LOOP ( 'NONE', ( #7303, #7001, #11986, #3267 ) ) ;
#6188 = ORIENTED_EDGE ( 'NONE', *, *, #2950, .F. ) ;
#6189 = FACE_OUTER_BOUND ( 'NONE', #12860, .T. ) ;
#6190 = CARTESIAN_POINT ( 'NONE',  ( -9.844122869686341204, -91.60173160181895469, -1.011447867193920658 ) ) ;
#6191 = DIRECTION ( 'NONE',  ( -0.6000000000000001998, -0.7999999999999999334, 0.000000000000000000 ) ) ;
#6192 = CIRCLE ( 'NONE', #146, 2.000000000000003997 ) ;
#6193 = DIRECTION ( 'NONE',  ( 0.000000000000000000, 0.000000000000000000, 1.000000000000000000 ) ) ;
#6194 = DIRECTION ( 'NONE',  ( -1.000000000000000000, 0.000000000000000000, 0.000000000000000000 ) ) ;
#6195 = EDGE_CURVE ( 'NONE', #3082, #7032, #13769, .T. ) ;
#6196 = CARTESIAN_POINT ( 'NONE',  ( 4.861079856844285452, -110.7705047426206306, -4.116395442951102268 ) ) ;
#6197 = CARTESIAN_POINT ( 'NONE',  ( -9.115242551282449313, -73.26725378407866174, -4.373789832702658309 ) ) ;
#6198 = DIRECTION ( 'NONE',  ( -1.000000000000000000, 0.000000000000000000, 0.000000000000000000 ) ) ;
#6199 = VECTOR ( 'NONE', #9099, 999.9999999999998863 ) ;
#6200 = ORIENTED_EDGE ( 'NONE', *, *, #11349, .T. ) ;
#6201 = ORIENTED_EDGE ( 'NONE', *, *, #4372, .F. ) ;
#6202 = EDGE_CURVE ( 'NONE', #750, #12212, #8768, .T. ) ;
#6203 = ADVANCED_FACE ( 'NONE', ( #2458 ), #168, .T. ) ;
#6204 = DIRECTION ( 'NONE',  ( 6.158143864569485777E-17, 2.736152283717910599E-16, -1.000000000000000000 ) ) ;
#6205 = ORIENTED_EDGE ( 'NONE', *, *, #5303, .T. ) ;
#6206 = CARTESIAN_POINT ( 'NONE',  ( 14.20591609908152009, -14.75994833063034761, -4.336808689942017736E-15 ) ) ;
#6207 = CARTESIAN_POINT ( 'NONE',  ( 3.178328602730291941, -98.49082012759913596, 7.173849163080390667 ) ) ;
#6208 = CARTESIAN_POINT ( 'NONE',  ( 0.5048931899926654143, -158.0606060600380829, 1.721373026807350604 ) ) ;
#6209 = DIRECTION ( 'NONE',  ( -0.8907235428302473501, -0.4545454545454531425, 0.000000000000000000 ) ) ;
#6210 = CARTESIAN_POINT ( 'NONE',  ( -10.69346802281033959, 21.32451227372186864, -21.38693604562068984 ) ) ;
#6211 = CARTESIAN_POINT ( 'NONE',  ( -32.72727272727271952, 135.1423002281142089, -2.500000000000000000 ) ) ;
#6212 = EDGE_CURVE ( 'NONE', #13265, #4522, #3367, .T. ) ;
#6213 = CARTESIAN_POINT ( 'NONE',  ( 25.00000000000002132, -99.74063674767212717, -4.228074540580630369 ) ) ;
#6214 = DIRECTION ( 'NONE',  ( 1.000000000000000000, 0.000000000000000000, 0.000000000000000000 ) ) ;
#6215 = LINE ( 'NONE', #879, #12380 ) ;
#6216 = EDGE_CURVE ( 'NONE', #13042, #7777, #5672, .T. ) ;
#6217 = EDGE_LOOP ( 'NONE', ( #5919, #4489, #12888, #8746 ) ) ;
#6218 = DIRECTION ( 'NONE',  ( -0.6000000000000001998, 0.7999999999999998224, 0.000000000000000000 ) ) ;
#6219 = DIRECTION ( 'NONE',  ( 1.000000000000000000, 1.850371707708595549E-15, 0.000000000000000000 ) ) ;
#6220 = CARTESIAN_POINT ( 'NONE',  ( -4.246087656249755149, -68.90909090942406579, 1.771789674518133184 ) ) ;
#6221 = ORIENTED_EDGE ( 'NONE', *, *, #7380, .F. ) ;
#6222 = ORIENTED_EDGE ( 'NONE', *, *, #8733, .T. ) ;
#6223 = PLANE ( 'NONE',  #11746 ) ;
#6224 = CARTESIAN_POINT ( 'NONE',  ( -35.06230589874905235, 106.5835921350012825, 2.499999999999999556 ) ) ;
#6225 = CARTESIAN_POINT ( 'NONE',  ( 10.82460162405762460, -71.99999999999998579, 2.658570984654982539 ) ) ;
#6226 = CARTESIAN_POINT ( 'NONE',  ( 1.916816365364574892, -124.8181818181859057, 4.196942880910825124 ) ) ;
#6227 = DIRECTION ( 'NONE',  ( 0.000000000000000000, 0.000000000000000000, 1.000000000000000000 ) ) ;
#6228 = CARTESIAN_POINT ( 'NONE',  ( -10.69346802281035025, 49.59884612375012125, -1.484741062544533711E-15 ) ) ;
#6229 = LINE ( 'NONE', #8255, #5902 ) ;
#6230 = CARTESIAN_POINT ( 'NONE',  ( 8.385254915620292238, 50.40394642271930792, 9.355740606675297531E-16 ) ) ;
#6231 = ORIENTED_EDGE ( 'NONE', *, *, #9104, .T. ) ;
#6232 = ORIENTED_EDGE ( 'NONE', *, *, #6039, .T. ) ;
#6233 = CARTESIAN_POINT ( 'NONE',  ( 8.385254915620294014, -12.94488700934118341, 1.052073721316228892E-15 ) ) ;
#6234 = CARTESIAN_POINT ( 'NONE',  ( 12.99553232110413781, 67.62342244460847951, 3.182987412051231379E-15 ) ) ;
#6235 = CARTESIAN_POINT ( 'NONE',  ( 10.69346802281035025, 30.74929022373127196, -21.38693604562068984 ) ) ;
#6236 = CARTESIAN_POINT ( 'NONE',  ( 23.44929957547844879, 14.76842309468663572, 2.500000000000003553 ) ) ;
#6237 = CARTESIAN_POINT ( 'NONE',  ( 1.055520991492275407, -150.0189090233429567, 1.640041038016263331 ) ) ;
#6238 = VECTOR ( 'NONE', #1764, 1000.000000000000000 ) ;
#6239 = CARTESIAN_POINT ( 'NONE',  ( 26.69171018101576465, -19.44228176112429551, -2.500000000000004441 ) ) ;
#6240 = CIRCLE ( 'NONE', #8909, 2.500000000000002220 ) ;
#6241 = VERTEX_POINT ( 'NONE', #11856 ) ;
#6242 = ORIENTED_EDGE ( 'NONE', *, *, #9996, .F. ) ;
#6243 = VERTEX_POINT ( 'NONE', #9757 ) ;
#6244 = FACE_OUTER_BOUND ( 'NONE', #8092, .T. ) ;
#6245 = AXIS2_PLACEMENT_3D ( 'NONE', #414, #2568, #6907 ) ;
#6246 = ORIENTED_EDGE ( 'NONE', *, *, #802, .T. ) ;
#6247 = EDGE_LOOP ( 'NONE', ( #13723, #7947, #2124, #10124 ) ) ;
#6248 = CARTESIAN_POINT ( 'NONE',  ( -10.69346802281035202, 77.87317997377837742, -2.801244458071077041E-15 ) ) ;
#6249 = EDGE_LOOP ( 'NONE', ( #1265, #6415, #4530, #7921 ) ) ;
#6250 = DIRECTION ( 'NONE',  ( -6.158143864569485777E-17, -2.736152283717910599E-16, 1.000000000000000000 ) ) ;
#6251 = CARTESIAN_POINT ( 'NONE',  ( -8.385254915620292238, 43.60378069071538221, -1.180893628524435759E-15 ) ) ;
#6252 = LINE ( 'NONE', #3087, #13715 ) ;
#6253 = LINE ( 'NONE', #4924, #12914 ) ;
#6254 = CARTESIAN_POINT ( 'NONE',  ( -1.392812481782718104, -130.7247055227911972, 3.705400635335541537 ) ) ;
#6255 = FACE_OUTER_BOUND ( 'NONE', #1055, .T. ) ;
#6256 = CIRCLE ( 'NONE', #8958, 2.500000000000002220 ) ;
#6257 = ORIENTED_EDGE ( 'NONE', *, *, #7321, .T. ) ;
#6258 = CARTESIAN_POINT ( 'NONE',  ( 0.8861126034330837342, -145.6297630941380987, -2.175407028858133085 ) ) ;
#6259 = CARTESIAN_POINT ( 'NONE',  ( -2.517691654963332357E-15, 90.00000000000000000, -1.589271161308885878E-16 ) ) ;
#6260 = EDGE_CURVE ( 'NONE', #4145, #3627, #9262, .T. ) ;
#6261 = CARTESIAN_POINT ( 'NONE',  ( 15.29705854078137861, 38.52236939141059935, 30.59411708156277498 ) ) ;
#6262 = ADVANCED_FACE ( 'NONE', ( #7712 ), #7914, .F. ) ;
#6263 = FACE_OUTER_BOUND ( 'NONE', #10320, .T. ) ;
#6264 = CARTESIAN_POINT ( 'NONE',  ( -4.736736781129390117, -106.7560981827712965, 4.922394428301823943 ) ) ;
#6265 = AXIS2_PLACEMENT_3D ( 'NONE', #7313, #12522, #6140 ) ;
#6266 = CARTESIAN_POINT ( 'NONE',  ( -32.72727272727271952, 135.1423002281142089, 0.5000000000000000000 ) ) ;
#6267 = ADVANCED_FACE ( 'NONE', ( #6594 ), #9824, .T. ) ;
#6268 = DIRECTION ( 'NONE',  ( -2.797435172181481150E-17, 1.000000000000000000, -1.765856845898762549E-18 ) ) ;
#6269 = EDGE_CURVE ( 'NONE', #9012, #3902, #9933, .T. ) ;
#6270 = CARTESIAN_POINT ( 'NONE',  ( 15.29705854078139637, 0.8232575913729167638, 1.873561326908939829E-15 ) ) ;
#6271 = AXIS2_PLACEMENT_3D ( 'NONE', #244, #3445, #5484 ) ;
#6272 = DIRECTION ( 'NONE',  ( 0.8000000000000008216, 0.5999999999999988676, -4.163336342344329138E-15 ) ) ;
#6273 = CARTESIAN_POINT ( 'NONE',  ( 25.00000000000000355, 120.0000000000000142, 7.500000000000000000 ) ) ;
#6274 = DIRECTION ( 'NONE',  ( 1.000000000000000000, 0.000000000000000000, 0.000000000000000000 ) ) ;
#6275 = CARTESIAN_POINT ( 'NONE',  ( -8.385254915620294014, 12.70483462268159869, -2.243491919447391838E-17 ) ) ;
#6276 = DIRECTION ( 'NONE',  ( 0.000000000000000000, 1.000000000000000000, 1.734723475976805615E-16 ) ) ;
#6277 = AXIS2_PLACEMENT_3D ( 'NONE', #3352, #2167, #10654 ) ;
#6278 = CARTESIAN_POINT ( 'NONE',  ( -11.42080557900780668, -157.8181818179944855, 3.873507862836679916 ) ) ;
#6279 = AXIS2_PLACEMENT_3D ( 'NONE', #12945, #4651, #3308 ) ;
#6280 = ORIENTED_EDGE ( 'NONE', *, *, #11827, .T. ) ;
#6281 = CIRCLE ( 'NONE', #8728, 67.49999999999997158 ) ;
#6282 = CARTESIAN_POINT ( 'NONE',  ( -12.99579180576517246, -11.31471392308272428, 25.99158361153033070 ) ) ;
#6283 = ORIENTED_EDGE ( 'NONE', *, *, #7820, .T. ) ;
#6284 = CARTESIAN_POINT ( 'NONE',  ( -8.385254915620295790, 90.00000000000000000, -1.589271161308885878E-16 ) ) ;
#6285 = DIRECTION ( 'NONE',  ( 1.000000000000000000, 0.000000000000000000, 0.000000000000000000 ) ) ;
#6286 = CARTESIAN_POINT ( 'NONE',  ( -35.00000000000000000, -35.00000000000000000, 7.500000000000000000 ) ) ;
#6287 = CARTESIAN_POINT ( 'NONE',  ( 12.87330105402722680, -111.7272727272711705, -6.772701765862029433 ) ) ;
#6288 = ADVANCED_FACE ( 'NONE', ( #1622 ), #13224, .T. ) ;
#6289 = CARTESIAN_POINT ( 'NONE',  ( 0.6173387890061909911, 90.00000000000000000, -4.961742921553712549 ) ) ;
#6290 = CARTESIAN_POINT ( 'NONE',  ( 8.385254915620290461, 50.40394642271930081, 16.77050983124059158 ) ) ;
#6291 = CIRCLE ( 'NONE', #6954, 12.49999999999999289 ) ;
#6292 = CARTESIAN_POINT ( 'NONE',  ( -2.504065471750553911E-13, 90.00000000000000000, -3.100119530583082101E-14 ) ) ;
#6293 = CARTESIAN_POINT ( 'NONE',  ( -11.81226048336476886, -40.00941361824966691, -1.305282905288380184E-15 ) ) ;
#6294 = ORIENTED_EDGE ( 'NONE', *, *, #11295, .T. ) ;
#6295 = CIRCLE ( 'NONE', #258, 2.000000000000007105 ) ;
#6296 = APPLICATION_CONTEXT ( 'automotive_design' ) ;
#6297 = CARTESIAN_POINT ( 'NONE',  ( -8.842511989038502662, -90.40394009946363951, -0.01791039437029070397 ) ) ;
#6298 = AXIS2_PLACEMENT_3D ( 'NONE', #6578, #5597, #4400 ) ;
#6299 = AXIS2_PLACEMENT_3D ( 'NONE', #1607, #9114, #9042 ) ;
#6300 = ORIENTED_EDGE ( 'NONE', *, *, #13630, .T. ) ;
#6301 = FACE_OUTER_BOUND ( 'NONE', #4767, .T. ) ;
#6302 = CARTESIAN_POINT ( 'NONE',  ( -36.36363636363635976, 142.2680885707561629, -0.5000000000000000000 ) ) ;
#6303 = EDGE_CURVE ( 'NONE', #12930, #3310, #4919, .T. ) ;
#6304 = DIRECTION ( 'NONE',  ( -6.158143864569485777E-17, -2.736152283717910599E-16, 1.000000000000000000 ) ) ;
#6305 = DIRECTION ( 'NONE',  ( 1.000000000000000000, 0.000000000000000000, 0.000000000000000000 ) ) ;
#6306 = DIRECTION ( 'NONE',  ( -1.000000000000000000, 0.000000000000000000, 0.000000000000000000 ) ) ;
#6307 = CARTESIAN_POINT ( 'NONE',  ( 4.330127018922191873, 90.00000000000000000, 0.5000000000000000000 ) ) ;
#6308 = AXIS2_PLACEMENT_3D ( 'NONE', #97, #8634, #5539 ) ;
#6309 = ORIENTED_EDGE ( 'NONE', *, *, #12128, .F. ) ;
#6310 = CARTESIAN_POINT ( 'NONE',  ( -2.010743657263654653E-15, 71.87811454074363837, -1.269264606320675724E-16 ) ) ;
#6311 = FACE_OUTER_BOUND ( 'NONE', #2015, .T. ) ;
#6312 = VERTEX_POINT ( 'NONE', #524 ) ;
#6313 = CARTESIAN_POINT ( 'NONE',  ( 8.627629343136117512, -71.90909090909211443, 5.462837922541618596 ) ) ;
#6314 = VERTEX_POINT ( 'NONE', #11366 ) ;
#6315 = CARTESIAN_POINT ( 'NONE',  ( 41.49999999999999289, 98.00000000000001421, 7.500000000000000000 ) ) ;
#6316 = DIRECTION ( 'NONE',  ( -1.000000000000000000, 0.000000000000000000, 0.000000000000000000 ) ) ;
#6317 = CARTESIAN_POINT ( 'NONE',  ( -10.35394582475455394, -72.00000000000014211, -3.762420212848085033 ) ) ;
#6318 = CARTESIAN_POINT ( 'NONE',  ( -34.79486456029760433, 106.9754367860671778, -2.376147960742915455 ) ) ;
#6319 = CARTESIAN_POINT ( 'NONE',  ( 10.69346802281034492, 68.44840202376897764, 1.228280763400934348E-15 ) ) ;
#6320 = CARTESIAN_POINT ( 'NONE',  ( -0.3211315587227348556, -154.7330882371165046, -1.606866635973652757 ) ) ;
#6321 = CARTESIAN_POINT ( 'NONE',  ( 1.958204620527036497E-15, -70.00000000000000000, 1.236099792129133461E-16 ) ) ;
#6322 = VERTEX_POINT ( 'NONE', #12287 ) ;
#6323 = EDGE_CURVE ( 'NONE', #10942, #10921, #7090, .T. ) ;
#6324 = ORIENTED_EDGE ( 'NONE', *, *, #1794, .T. ) ;
#6325 = VERTEX_POINT ( 'NONE', #2678 ) ;
#6326 = CARTESIAN_POINT ( 'NONE',  ( 48.00000000000000000, 120.0000000000000142, 2.500000000000000000 ) ) ;
#6327 = DIRECTION ( 'NONE',  ( -0.000000000000000000, -0.000000000000000000, -1.000000000000000000 ) ) ;
#6328 = B_SPLINE_CURVE_WITH_KNOTS ( 'NONE', 3,
 ( #10488, #6157, #5161, #4104, #7395, #5026, #9308, #2006, #11477, #8250, #12543, #12612, #6350, #13756, #2989, #10619 ),
 .UNSPECIFIED., .F., .F.,
 ( 4, 2, 2, 2, 2, 2, 2, 4 ),
 ( 0.000000000000000000, 0.003943481679486459703, 0.005915222519229688253, 0.007886963358972917670, 0.009858704198716145353, 0.01183044503845937477, 0.01380218587820260592, 0.01577392671794583534 ),
 .UNSPECIFIED. ) ;
#6329 = VERTEX_POINT ( 'NONE', #11163 ) ;
#6330 = CARTESIAN_POINT ( 'NONE',  ( -35.04450421339218025, 112.5597086678580609, 2.499999999999999556 ) ) ;
#6331 = CARTESIAN_POINT ( 'NONE',  ( -5.217808995651798121, -115.4128671718531223, -2.475508680495110525 ) ) ;
#6332 = AXIS2_PLACEMENT_3D ( 'NONE', #12039, #11764, #7683 ) ;
#6333 = DIRECTION ( 'NONE',  ( 0.9923485843107423543, 2.797833471351478217E-17, 0.1234677578012386562 ) ) ;
#6334 = CARTESIAN_POINT ( 'NONE',  ( 10.69381717166375267, 63.25855867215299355, 1.228320867585964984E-15 ) ) ;
#6335 = CARTESIAN_POINT ( 'NONE',  ( 12.99553232110414491, 20.49953269456136695, -25.99106464220827561 ) ) ;
#6336 = DIRECTION ( 'NONE',  ( -6.158143864569485777E-17, -2.736152283717910599E-16, 1.000000000000000000 ) ) ;
#6337 = EDGE_CURVE ( 'NONE', #4279, #2222, #8292, .T. ) ;
#6338 = DIRECTION ( 'NONE',  ( 1.000000000000000000, 0.000000000000000000, 0.000000000000000000 ) ) ;
#6339 = CARTESIAN_POINT ( 'NONE',  ( 10.69346802281034492, 68.44840202376897764, 0.000000000000000000 ) ) ;
#6340 = EDGE_CURVE ( 'NONE', #12494, #11430, #8145, .T. ) ;
#6341 = EDGE_CURVE ( 'NONE', #2641, #3641, #551, .T. ) ;
#6342 = ORIENTED_EDGE ( 'NONE', *, *, #1724, .T. ) ;
#6343 = DIRECTION ( 'NONE',  ( 0.000000000000000000, 0.000000000000000000, -1.000000000000000000 ) ) ;
#6344 = DIRECTION ( 'NONE',  ( -0.000000000000000000, -0.000000000000000000, -1.000000000000000000 ) ) ;
#6345 = CARTESIAN_POINT ( 'NONE',  ( 2.318285725469618086, -147.1038961039384674, 4.595794441991605694 ) ) ;
#6346 = ORIENTED_EDGE ( 'NONE', *, *, #1161, .T. ) ;
#6347 = CARTESIAN_POINT ( 'NONE',  ( 41.86252833142972918, 24.55922850786694056, 7.372574772901430151E-15 ) ) ;
#6348 = ORIENTED_EDGE ( 'NONE', *, *, #5490, .T. ) ;
#6349 = DIRECTION ( 'NONE',  ( -0.000000000000000000, -0.000000000000000000, -1.000000000000000000 ) ) ;
#6350 = CARTESIAN_POINT ( 'NONE',  ( 14.85082311557358103, -22.21562007816738316, -5.135570635274604001 ) ) ;
#6351 = CARTESIAN_POINT ( 'NONE',  ( 12.88103206736702511, -118.2727272727294121, 6.757986543075767294 ) ) ;
#6352 = DIRECTION ( 'NONE',  ( 1.000000000000000000, -0.000000000000000000, 0.000000000000000000 ) ) ;
#6353 = DIRECTION ( 'NONE',  ( -1.000000000000000000, -2.081668171172168119E-15, 0.000000000000000000 ) ) ;
#6354 = CYLINDRICAL_SURFACE ( 'NONE', #12250, 5.999999999999998224 ) ;
#6355 = CARTESIAN_POINT ( 'NONE',  ( 75.98647239440286683, -111.6214737678657087, 2.500000000000000000 ) ) ;
#6356 = EDGE_CURVE ( 'NONE', #12845, #357, #5444, .T. ) ;
#6357 = CARTESIAN_POINT ( 'NONE',  ( -34.25812584745457201, 108.1980041606221192, 0.000000000000000000 ) ) ;
#6358 = ADVANCED_FACE ( 'NONE', ( #9265 ), #787, .T. ) ;
#6359 = ORIENTED_EDGE ( 'NONE', *, *, #2253, .F. ) ;
#6360 = EDGE_CURVE ( 'NONE', #1890, #1745, #13582, .T. ) ;
#6361 = AXIS2_PLACEMENT_3D ( 'NONE', #2955, #7221, #11504 ) ;
#6362 = EDGE_CURVE ( 'NONE', #2145, #13485, #3646, .T. ) ;
#6363 = PRESENTATION_STYLE_ASSIGNMENT (( #10828 ) ) ;
#6364 = ORIENTED_EDGE ( 'NONE', *, *, #6885, .F. ) ;
#6365 = CYLINDRICAL_SURFACE ( 'NONE', #7409, 15.29705854078139105 ) ;
#6366 = DIRECTION ( 'NONE',  ( 0.000000000000000000, 0.000000000000000000, -1.000000000000000000 ) ) ;
#6367 = CARTESIAN_POINT ( 'NONE',  ( -15.29705854078139105, 29.09759144140119957, -3.799746640842329186E-15 ) ) ;
#6368 = AXIS2_PLACEMENT_3D ( 'NONE', #10683, #4038, #13885 ) ;
#6369 = CARTESIAN_POINT ( 'NONE',  ( 1.819477288719722585, -146.4205547847951152, 1.378398102139016368 ) ) ;
#6370 = ADVANCED_FACE ( 'NONE', ( #6383 ), #7350, .T. ) ;
#6371 = FACE_OUTER_BOUND ( 'NONE', #10804, .T. ) ;
#6372 = ORIENTED_EDGE ( 'NONE', *, *, #5341, .F. ) ;
#6373 = ORIENTED_EDGE ( 'NONE', *, *, #1444, .T. ) ;
#6374 = ORIENTED_EDGE ( 'NONE', *, *, #43, .F. ) ;
#6375 = EDGE_CURVE ( 'NONE', #6810, #2418, #724, .T. ) ;
#6376 = DIRECTION ( 'NONE',  ( -0.000000000000000000, 1.000000000000000000, -0.000000000000000000 ) ) ;
#6377 = CIRCLE ( 'NONE', #11539, 15.29705854078139282 ) ;
#6378 = CYLINDRICAL_SURFACE ( 'NONE', #5023, 8.385254915620292238 ) ;
#6379 = ORIENTED_EDGE ( 'NONE', *, *, #5228, .F. ) ;
#6380 = CARTESIAN_POINT ( 'NONE',  ( 4.840675591955164059, -75.54545454545383620, 8.982239580829949332 ) ) ;
#6381 = AXIS2_PLACEMENT_3D ( 'NONE', #3815, #11185, #1775 ) ;
#6382 = ORIENTED_EDGE ( 'NONE', *, *, #2173, .T. ) ;
#6383 = FACE_OUTER_BOUND ( 'NONE', #4484, .T. ) ;
#6384 = CARTESIAN_POINT ( 'NONE',  ( 32.61455173758670867, 25.38817907193537593, -2.499999999999992450 ) ) ;
#6385 = FACE_OUTER_BOUND ( 'NONE', #4397, .T. ) ;
#6386 = CARTESIAN_POINT ( 'NONE',  ( -2.504065471750553911E-13, 90.00000000000000000, -3.100119530583082101E-14 ) ) ;
#6387 = DIRECTION ( 'NONE',  ( 0.000000000000000000, 0.000000000000000000, 1.000000000000000000 ) ) ;
#6388 = CARTESIAN_POINT ( 'NONE',  ( 4.535930497296239317, -119.9429431484441722, 2.586521195913217053 ) ) ;
#6389 = DIRECTION ( 'NONE',  ( -1.000000000000000000, 0.000000000000000000, 0.000000000000000000 ) ) ;
#6390 = ORIENTED_EDGE ( 'NONE', *, *, #8223, .T. ) ;
#6391 = EDGE_LOOP ( 'NONE', ( #8, #11969 ) ) ;
#6392 = COLOUR_RGB ( '', 0.09019608, 0.27058824, 0.51372549) ;
#6393 = ORIENTED_EDGE ( 'NONE', *, *, #708, .F. ) ;
#6394 = B_SPLINE_CURVE_WITH_KNOTS ( 'NONE', 3,
 ( #4870, #9148, #8563, #6399 ),
 .UNSPECIFIED., .F., .F.,
 ( 4, 4 ),
 ( 0.03713967652845541478, 0.04074225392669963280 ),
 .UNSPECIFIED. ) ;
#6395 = AXIS2_PLACEMENT_3D ( 'NONE', #11847, #8554, #2171 ) ;
#6396 = CARTESIAN_POINT ( 'NONE',  ( -25.00000000000000355, 120.0000000000000142, 2.500000000000000000 ) ) ;
#6397 = EDGE_LOOP ( 'NONE', ( #5555, #11292, #6609, #7610 ) ) ;
#6398 = AXIS2_PLACEMENT_3D ( 'NONE', #12275, #6932, #6653 ) ;
#6399 = CARTESIAN_POINT ( 'NONE',  ( 24.37649275748779232, -100.0000000000000000, -7.500000000000000000 ) ) ;
#6400 = CARTESIAN_POINT ( 'NONE',  ( -3.621723652282179629, -105.2179775488178137, 6.003010775146917943 ) ) ;
#6401 = CARTESIAN_POINT ( 'NONE',  ( -39.99999999999999289, 120.0000000000000142, 2.500000000000000000 ) ) ;
#6402 = FACE_OUTER_BOUND ( 'NONE', #4423, .T. ) ;
#6403 = CARTESIAN_POINT ( 'NONE',  ( -42.16244658108818300, 105.4500712252157797, -2.500000000000000444 ) ) ;
#6404 = DIRECTION ( 'NONE',  ( -2.797435172181481150E-17, 1.000000000000000000, -1.765856845898762549E-18 ) ) ;
#6405 = TOROIDAL_SURFACE ( 'NONE', #10439, 77.99999999999997158, 2.000000000000000000 ) ;
#6406 = CARTESIAN_POINT ( 'NONE',  ( -6.726204760714091790, -75.54545454545716154, -7.481082188384119647 ) ) ;
#6407 = CARTESIAN_POINT ( 'NONE',  ( 25.00000000000001776, -99.86284836912254548, -4.640101051368624496 ) ) ;
#6408 = CARTESIAN_POINT ( 'NONE',  ( 34.99999999999958789, 1.104930248025249758E-13, -2.499999999999997335 ) ) ;
#6409 = ORIENTED_EDGE ( 'NONE', *, *, #1814, .F. ) ;
#6410 = AXIS2_PLACEMENT_3D ( 'NONE', #6801, #4692, #4773 ) ;
#6411 = DIRECTION ( 'NONE',  ( -0.000000000000000000, -0.000000000000000000, -1.000000000000000000 ) ) ;
#6412 = LINE ( 'NONE', #9703, #5584 ) ;
#6413 = EDGE_LOOP ( 'NONE', ( #4408, #11902, #13797 ) ) ;
#6414 = DIRECTION ( 'NONE',  ( -6.158143864569485777E-17, -2.736152283717910599E-16, 1.000000000000000000 ) ) ;
#6415 = ORIENTED_EDGE ( 'NONE', *, *, #2599, .T. ) ;
#6416 = CARTESIAN_POINT ( 'NONE',  ( -2.517691654963332357E-15, 90.00000000000000000, -1.589271161308885878E-16 ) ) ;
#6417 = ORIENTED_EDGE ( 'NONE', *, *, #13664, .F. ) ;
#6418 = DIRECTION ( 'NONE',  ( -6.158143864569485777E-17, -2.736152283717910599E-16, 1.000000000000000000 ) ) ;
#6419 = DIRECTION ( 'NONE',  ( -0.000000000000000000, -0.000000000000000000, -1.000000000000000000 ) ) ;
#6420 = ADVANCED_FACE ( 'NONE', ( #11509 ), #10391, .T. ) ;
#6421 = AXIS2_PLACEMENT_3D ( 'NONE', #5029, #9310, #12745 ) ;
#6422 = CARTESIAN_POINT ( 'NONE',  ( -4.364119526982408459, -68.90909090871591047, -1.457038019223346526 ) ) ;
#6423 = DIRECTION ( 'NONE',  ( -1.000000000000000000, -1.734723475976805517E-15, 0.000000000000000000 ) ) ;
#6424 = CYLINDRICAL_SURFACE ( 'NONE', #12707, 4.999999999999998224 ) ;
#6425 = CARTESIAN_POINT ( 'NONE',  ( 38.79999999999999716, 101.5999999999999943, 2.500000000000000000 ) ) ;
#6426 = DIRECTION ( 'NONE',  ( 1.000000000000000000, 0.000000000000000000, -0.000000000000000000 ) ) ;
#6427 = FACE_OUTER_BOUND ( 'NONE', #983, .T. ) ;
#6428 = ORIENTED_EDGE ( 'NONE', *, *, #5868, .T. ) ;
#6429 = EDGE_CURVE ( 'NONE', #9684, #6890, #759, .T. ) ;
#6430 = EDGE_CURVE ( 'NONE', #4098, #7192, #3893, .T. ) ;
#6431 = ORIENTED_EDGE ( 'NONE', *, *, #6303, .T. ) ;
#6432 = DIRECTION ( 'NONE',  ( 6.158143864569485777E-17, 2.736152283717910599E-16, -1.000000000000000000 ) ) ;
#6433 = EDGE_CURVE ( 'NONE', #11415, #5518, #4000, .T. ) ;
#6434 = CARTESIAN_POINT ( 'NONE',  ( 42.16244658108818300, 105.4500712252157655, 2.499999999999999556 ) ) ;
#6435 = DIRECTION ( 'NONE',  ( 1.000000000000000000, 0.000000000000000000, 0.000000000000000000 ) ) ;
#6436 = EDGE_CURVE ( 'NONE', #1633, #13463, #1114, .T. ) ;
#6437 = CARTESIAN_POINT ( 'NONE',  ( -9.876538000534836215, -71.62961015872004111, -2.126563546433114738 ) ) ;
#6438 = EDGE_CURVE ( 'NONE', #6908, #8462, #11639, .T. ) ;
#6439 = CARTESIAN_POINT ( 'NONE',  ( 0.000000000000000000, 71.01020514433645303, -2.500000000000000000 ) ) ;
#6440 = DIRECTION ( 'NONE',  ( -1.000000000000000000, 0.000000000000000000, 0.000000000000000000 ) ) ;
#6441 = VERTEX_POINT ( 'NONE', #4135 ) ;
#6442 = ORIENTED_EDGE ( 'NONE', *, *, #10554, .T. ) ;
#6443 = ORIENTED_EDGE ( 'NONE', *, *, #718, .F. ) ;
#6444 = ADVANCED_FACE ( 'NONE', ( #6189 ), #7157, .T. ) ;
#6445 = ORIENTED_EDGE ( 'NONE', *, *, #8930, .F. ) ;
#6446 = DIRECTION ( 'NONE',  ( -1.000000000000000000, 0.000000000000000000, 0.000000000000000000 ) ) ;
#6447 = ORIENTED_EDGE ( 'NONE', *, *, #2410, .T. ) ;
#6448 = CARTESIAN_POINT ( 'NONE',  ( 27.38873514654796537, -24.33759740261776017, -4.000000000000000000 ) ) ;
#6449 = FACE_OUTER_BOUND ( 'NONE', #5116, .T. ) ;
#6450 = CARTESIAN_POINT ( 'NONE',  ( -2.255225165641619345, -77.73185736634954424, -9.851628698357723479 ) ) ;
#6451 = ADVANCED_FACE ( 'NONE', ( #3083 ), #8283, .T. ) ;
#6452 = DIRECTION ( 'NONE',  ( 1.000000000000000000, 2.668805347656626185E-16, -0.000000000000000000 ) ) ;
#6453 = DIRECTION ( 'NONE',  ( -6.158143864569485777E-17, -2.736152283717910599E-16, 1.000000000000000000 ) ) ;
#6454 = CARTESIAN_POINT ( 'NONE',  ( -6.633121150698165991, -97.20333181108198062, -4.463170841960692137 ) ) ;
#6455 = DIRECTION ( 'NONE',  ( 0.9960067511297464593, -0.08927794634716622324, 6.802837160686558945E-17 ) ) ;
#6456 = ORIENTED_EDGE ( 'NONE', *, *, #4838, .T. ) ;
#6457 = VERTEX_POINT ( 'NONE', #10516 ) ;
#6458 = EDGE_LOOP ( 'NONE', ( #11269, #13201 ) ) ;
#6459 = AXIS2_PLACEMENT_3D ( 'NONE', #6109, #10376, #9328 ) ;
#6460 = TOROIDAL_SURFACE ( 'NONE', #9595, 42.00000000000001421, 2.000000000000000000 ) ;
#6461 = DIRECTION ( 'NONE',  ( -2.797435172181481150E-17, 1.000000000000000000, -1.765856845898762549E-18 ) ) ;
#6462 = LINE ( 'NONE', #166, #9192 ) ;
#6463 = VERTEX_POINT ( 'NONE', #5188 ) ;
#6464 = CARTESIAN_POINT ( 'NONE',  ( 34.66997162884352690, 21.14050806081579736, 2.500000000000005773 ) ) ;
#6465 = CARTESIAN_POINT ( 'NONE',  ( 12.99553232110413958, 39.34908859458022334, -25.99106464220826851 ) ) ;
#6466 = CARTESIAN_POINT ( 'NONE',  ( 25.00000000000000355, 120.0000000000000142, -7.500000000000000000 ) ) ;
#6467 = CYLINDRICAL_SURFACE ( 'NONE', #5808, 9.000000000008999024 ) ;
#6468 = LINE ( 'NONE', #8305, #7198 ) ;
#6469 = CARTESIAN_POINT ( 'NONE',  ( -9.860966656292097454, -69.99999999999948841, -1.730751479146293903 ) ) ;
#6470 = EDGE_CURVE ( 'NONE', #3638, #13779, #5784, .T. ) ;
#6471 = CARTESIAN_POINT ( 'NONE',  ( 2.680497156733089970, -80.99999999999992895, -9.800765866881897992 ) ) ;
#6472 = AXIS2_PLACEMENT_3D ( 'NONE', #129, #4380, #60 ) ;
#6473 = CARTESIAN_POINT ( 'NONE',  ( -8.385254915620295790, -15.56949922734665748, 16.77050983124058448 ) ) ;
#6474 = DIRECTION ( 'NONE',  ( -0.000000000000000000, -0.000000000000000000, -1.000000000000000000 ) ) ;
#6475 = AXIS2_PLACEMENT_3D ( 'NONE', #5206, #13804, #1007 ) ;
#6476 = APPLICATION_CONTEXT ( 'automotive_design' ) ;
#6477 = CYLINDRICAL_SURFACE ( 'NONE', #5828, 9.000000000008999024 ) ;
#6478 = CARTESIAN_POINT ( 'NONE',  ( -35.00000000000000000, 25.00000000000000000, 7.500000000000000000 ) ) ;
#6479 = VERTEX_POINT ( 'NONE', #9477 ) ;
#6480 = EDGE_LOOP ( 'NONE', ( #6040, #13390, #7125, #3914, #5058, #13238 ) ) ;
#6481 = CARTESIAN_POINT ( 'NONE',  ( -35.00000000000000000, -4.286263797015736496E-15, 4.000000000000000000 ) ) ;
#6482 = AXIS2_PLACEMENT_3D ( 'NONE', #8227, #3099, #7368 ) ;
#6483 = VERTEX_POINT ( 'NONE', #12710 ) ;
#6484 = FACE_OUTER_BOUND ( 'NONE', #6187, .T. ) ;
#6485 = ORIENTED_EDGE ( 'NONE', *, *, #2691, .T. ) ;
#6486 = CYLINDRICAL_SURFACE ( 'NONE', #12886, 14.99999999999999112 ) ;
#6487 = AXIS2_PLACEMENT_3D ( 'NONE', #11253, #8854, #4724 ) ;
#6488 = CARTESIAN_POINT ( 'NONE',  ( -15.29705854078139815, 0.8232575913729157646, 30.59411708156277854 ) ) ;
#6489 = CARTESIAN_POINT ( 'NONE',  ( 15.29705854078139282, 74.33491362204294717, 1.740418857596141236E-15 ) ) ;
#6490 = DIRECTION ( 'NONE',  ( 0.8907235428302465730, 0.4545454545454549189, -0.000000000000000000 ) ) ;
#6491 = FACE_OUTER_BOUND ( 'NONE', #7383, .T. ) ;
#6492 = CARTESIAN_POINT ( 'NONE',  ( 39.31542348013558552, 101.3376241895501977, 2.435478634890659855 ) ) ;
#6493 = DIRECTION ( 'NONE',  ( -0.000000000000000000, -0.000000000000000000, -1.000000000000000000 ) ) ;
#6494 = CIRCLE ( 'NONE', #10947, 5.999999999999998224 ) ;
#6495 = CARTESIAN_POINT ( 'NONE',  ( 15.29705854078138749, 17.78624592198638155, 3.746698755667521623E-15 ) ) ;
#6496 = CIRCLE ( 'NONE', #1575, 8.385254915620294014 ) ;
#6497 = EDGE_CURVE ( 'NONE', #8031, #4461, #11934, .T. ) ;
#6498 = CIRCLE ( 'NONE', #12571, 2.000000000000003109 ) ;
#6499 = EDGE_LOOP ( 'NONE', ( #5721, #9937, #70, #9960, #13512 ) ) ;
#6500 = AXIS2_PLACEMENT_3D ( 'NONE', #9253, #710, #13774 ) ;
#6501 = FILL_AREA_STYLE ('',( #13896 ) ) ;
#6502 = ORIENTED_EDGE ( 'NONE', *, *, #686, .F. ) ;
#6503 = CARTESIAN_POINT ( 'NONE',  ( -12.99553232110414314, 67.62342244460847951, 25.99106464220826496 ) ) ;
#6504 = CIRCLE ( 'NONE', #5845, 15.29705854078138749 ) ;
#6505 = CARTESIAN_POINT ( 'NONE',  ( 0.000000000000000000, 71.01020514433645303, 0.5000000000000000000 ) ) ;
#6506 = DIRECTION ( 'NONE',  ( -0.000000000000000000, -0.000000000000000000, -1.000000000000000000 ) ) ;
#6507 = CYLINDRICAL_SURFACE ( 'NONE', #8127, 14.99999999999998934 ) ;
#6508 = CARTESIAN_POINT ( 'NONE',  ( 15.29705854078138749, 10.24803554138234496, 3.746698755667521623E-15 ) ) ;
#6509 = ORIENTED_EDGE ( 'NONE', *, *, #5651, .T. ) ;
#6510 = ADVANCED_FACE ( 'NONE', ( #3145 ), #10370, .F. ) ;
#6511 = TOROIDAL_SURFACE ( 'NONE', #7619, 22.99999999999999289, 2.000000000000000000 ) ;
#6512 = EDGE_CURVE ( 'NONE', #11768, #11894, #103, .T. ) ;
#6513 = CIRCLE ( 'NONE', #8313, 15.29705854078139637 ) ;
#6514 = AXIS2_PLACEMENT_3D ( 'NONE', #9489, #1845, #2898 ) ;
#6515 = EDGE_CURVE ( 'NONE', #7693, #11081, #13328, .T. ) ;
#6516 = ORIENTED_EDGE ( 'NONE', *, *, #13419, .T. ) ;
#6517 = ORIENTED_EDGE ( 'NONE', *, *, #2737, .T. ) ;
#6518 = ORIENTED_EDGE ( 'NONE', *, *, #8155, .F. ) ;
#6519 = DIRECTION ( 'NONE',  ( 0.000000000000000000, 0.000000000000000000, 1.000000000000000000 ) ) ;
#6520 = DIRECTION ( 'NONE',  ( 1.000000000000000000, 0.000000000000000000, 0.000000000000000000 ) ) ;
#6521 = CARTESIAN_POINT ( 'NONE',  ( -3.108119021657300696, -77.10324913307979955, -9.630131037565234919 ) ) ;
#6522 = AXIS2_PLACEMENT_3D ( 'NONE', #12836, #8868, #9588 ) ;
#6523 = CARTESIAN_POINT ( 'NONE',  ( 39.64464840659818634, 101.1283747906780803, -2.297097423097429925 ) ) ;
#6524 = CARTESIAN_POINT ( 'NONE',  ( 4.230699918504775781, 91.18539124371000071, -2.666380740812164696 ) ) ;
#6525 = CARTESIAN_POINT ( 'NONE',  ( 1.140958104747115343, -80.62156175248728118, 9.984774867419227817 ) ) ;
#6526 = PLANE ( 'NONE',  #812 ) ;
#6527 = ORIENTED_EDGE ( 'NONE', *, *, #211, .F. ) ;
#6528 = ORIENTED_EDGE ( 'NONE', *, *, #458, .F. ) ;
#6529 = EDGE_CURVE ( 'NONE', #11270, #9012, #384, .T. ) ;
#6530 = VERTEX_POINT ( 'NONE', #7209 ) ;
#6531 = EDGE_CURVE ( 'NONE', #12400, #576, #8371, .T. ) ;
#6532 = EDGE_CURVE ( 'NONE', #5991, #8546, #5040, .T. ) ;
#6533 = AXIS2_PLACEMENT_3D ( 'NONE', #9133, #5986, #12072 ) ;
#6534 = CARTESIAN_POINT ( 'NONE',  ( 15.29705854078138927, 29.09759144140119957, 1.823632900916640086E-15 ) ) ;
#6535 = DIRECTION ( 'NONE',  ( -6.158143864569485777E-17, -2.736152283717910599E-16, 1.000000000000000000 ) ) ;
#6536 = ORIENTED_EDGE ( 'NONE', *, *, #11349, .F. ) ;
#6537 = CARTESIAN_POINT ( 'NONE',  ( -23.64268088454699779, -97.00000000000000000, 0.000000000000000000 ) ) ;
#6538 = CARTESIAN_POINT ( 'NONE',  ( -10.69346802281034137, 59.02362407375952102, -21.38693604562068984 ) ) ;
#6539 = CARTESIAN_POINT ( 'NONE',  ( 10.69381717166375623, 6.709890972096427042, 1.299272810468638199E-15 ) ) ;
#6540 = CARTESIAN_POINT ( 'NONE',  ( -39.99999999999999289, 100.0000000000000000, -0.5000000000000000000 ) ) ;
#6541 = CARTESIAN_POINT ( 'NONE',  ( -0.3668613529521884686, -160.9696969702431488, 1.703459722496312612 ) ) ;
#6542 = CARTESIAN_POINT ( 'NONE',  ( -9.807291687911792621, -69.33333333333621340, -2.012068907120004635 ) ) ;
#6543 = CARTESIAN_POINT ( 'NONE',  ( 10.69346802281034314, -16.37459952631584059, 21.38693604562069694 ) ) ;
#6544 = CARTESIAN_POINT ( 'NONE',  ( -2.517691654963332357E-15, 90.00000000000000000, -1.589271161308885878E-16 ) ) ;
#6545 = VERTEX_POINT ( 'NONE', #11165 ) ;
#6546 = CARTESIAN_POINT ( 'NONE',  ( 1.387778780781445676E-14, -100.0000000000000000, 0.000000000000000000 ) ) ;
#6547 = VERTEX_POINT ( 'NONE', #12147 ) ;
#6548 = AXIS2_PLACEMENT_3D ( 'NONE', #4436, #9998, #2339 ) ;
#6549 = EDGE_CURVE ( 'NONE', #297, #13779, #5689, .T. ) ;
#6550 = DIRECTION ( 'NONE',  ( 1.000000000000000000, 0.000000000000000000, 0.000000000000000000 ) ) ;
#6551 = DIRECTION ( 'NONE',  ( -1.000000000000000000, 0.000000000000000000, 0.000000000000000000 ) ) ;
#6552 = ORIENTED_EDGE ( 'NONE', *, *, #13831, .F. ) ;
#6553 = CIRCLE ( 'NONE', #1404, 1.999999999999998890 ) ;
#6554 = CARTESIAN_POINT ( 'NONE',  ( 8.385254915620292238, -12.94488700934118341, 1.052073721316228694E-15 ) ) ;
#6555 = VERTEX_POINT ( 'NONE', #11492 ) ;
#6556 = CARTESIAN_POINT ( 'NONE',  ( -10.69381717166375623, 72.68333662216238622, -1.566311632108520979E-15 ) ) ;
#6557 = CARTESIAN_POINT ( 'NONE',  ( -12.99579180576516535, 54.65873172698324112, -25.99158361153033425 ) ) ;
#6558 = CARTESIAN_POINT ( 'NONE',  ( 34.58386302044579708, 107.3580618547655803, -2.150514425741560931 ) ) ;
#6559 = DIRECTION ( 'NONE',  ( 0.000000000000000000, 0.000000000000000000, 1.000000000000000000 ) ) ;
#6560 = CARTESIAN_POINT ( 'NONE',  ( 15.29705854078138749, 10.24803554138234496, 1.856918518244839783E-15 ) ) ;
#6561 = CARTESIAN_POINT ( 'NONE',  ( 12.99579180576517423, -20.73949187309215247, 0.000000000000000000 ) ) ;
#6562 = CARTESIAN_POINT ( 'NONE',  ( -2.517691654963332357E-15, 90.00000000000000000, -1.589271161308885878E-16 ) ) ;
#6563 = AXIS2_PLACEMENT_3D ( 'NONE', #6919, #4832, #9108 ) ;
#6564 = DIRECTION ( 'NONE',  ( 1.000000000000000000, -1.850371707708595154E-15, 0.000000000000000000 ) ) ;
#6565 = EDGE_LOOP ( 'NONE', ( #5904, #8896, #5184, #12859, #523, #13500, #5174, #12286, #4861 ) ) ;
#6566 = ORIENTED_EDGE ( 'NONE', *, *, #12510, .T. ) ;
#6567 = DIRECTION ( 'NONE',  ( -1.000000000000000000, 0.000000000000000000, 0.000000000000000000 ) ) ;
#6568 = CARTESIAN_POINT ( 'NONE',  ( 21.34086416022640265, 21.53318388236929692, -2.499999999999994671 ) ) ;
#6569 = DIRECTION ( 'NONE',  ( -1.000000000000000000, 0.000000000000000000, 0.000000000000000000 ) ) ;
#6570 = UNCERTAINTY_MEASURE_WITH_UNIT (LENGTH_MEASURE( 1.000000000000000082E-05 ), #12413, 'distance_accuracy_value', 'NONE');
#6571 = CARTESIAN_POINT ( 'NONE',  ( -0.6173387890061953209, 79.99058638175036151, 4.961742921553712549 ) ) ;
#6572 = CIRCLE ( 'NONE', #12647, 22.49999999999999289 ) ;
#6573 = ORIENTED_EDGE ( 'NONE', *, *, #6438, .T. ) ;
#6574 = ORIENTED_EDGE ( 'NONE', *, *, #4372, .T. ) ;
#6575 = AXIS2_PLACEMENT_3D ( 'NONE', #12470, #2854, #9309 ) ;
#6576 = LINE ( 'NONE', #2230, #10305 ) ;
#6577 = VERTEX_POINT ( 'NONE', #2537 ) ;
#6578 = CARTESIAN_POINT ( 'NONE',  ( 34.99999999999958789, 1.091249486606660213E-13, 2.500000000000000000 ) ) ;
#6579 = AXIS2_PLACEMENT_3D ( 'NONE', #9031, #12110, #13343 ) ;
#6580 = FACE_OUTER_BOUND ( 'NONE', #8942, .T. ) ;
#6581 = DIRECTION ( 'NONE',  ( 1.000000000000000000, 0.000000000000000000, 0.000000000000000000 ) ) ;
#6582 = DIRECTION ( 'NONE',  ( -2.668805347656626185E-16, 1.000000000000000000, 0.000000000000000000 ) ) ;
#6583 = CARTESIAN_POINT ( 'NONE',  ( 53.56517978609545594, 2.618988451796029349, -2.499999999999997335 ) ) ;
#6584 = CARTESIAN_POINT ( 'NONE',  ( -2.434338757227561434, -101.9345656283768022, -7.012440599860332746 ) ) ;
#6585 = CARTESIAN_POINT ( 'NONE',  ( -10.00000000000000711, 139.9999999999999716, -2.500000000000000000 ) ) ;
#6586 = ORIENTED_EDGE ( 'NONE', *, *, #13626, .F. ) ;
#6587 = AXIS2_PLACEMENT_3D ( 'NONE', #12837, #11761, #4321 ) ;
#6588 = VERTEX_POINT ( 'NONE', #1882 ) ;
#6589 = ORIENTED_EDGE ( 'NONE', *, *, #11075, .T. ) ;
#6590 = AXIS2_PLACEMENT_3D ( 'NONE', #5093, #3905, #11201 ) ;
#6591 = CIRCLE ( 'NONE', #580, 22.99999999999999645 ) ;
#6592 = CARTESIAN_POINT ( 'NONE',  ( -39.06230589874905235, 109.5835921350012683, -2.499999999999999556 ) ) ;
#6593 = ORIENTED_EDGE ( 'NONE', *, *, #1914, .F. ) ;
#6594 = FACE_OUTER_BOUND ( 'NONE', #733, .T. ) ;
#6595 =( NAMED_UNIT ( * ) SI_UNIT ( $, .STERADIAN. ) SOLID_ANGLE_UNIT ( ) );
#6596 = CARTESIAN_POINT ( 'NONE',  ( -8.385254915620290461, 59.82872437272870769, -16.77050983124058448 ) ) ;
#6597 = ADVANCED_FACE ( 'NONE', ( #1624 ), #8995, .T. ) ;
#6598 = DIRECTION ( 'NONE',  ( 1.000000000000000000, 0.000000000000000000, 0.000000000000000000 ) ) ;
#6599 = CARTESIAN_POINT ( 'NONE',  ( 50.48962708925064646, 14.39101985375337556, -2.499999999999993783 ) ) ;
#6600 = EDGE_CURVE ( 'NONE', #13800, #4911, #6142, .T. ) ;
#6601 = CARTESIAN_POINT ( 'NONE',  ( -0.6121604151423207796, -166.5454546257185768, -9.081467143786552398 ) ) ;
#6602 = EDGE_CURVE ( 'NONE', #1315, #10942, #7247, .T. ) ;
#6603 = CARTESIAN_POINT ( 'NONE',  ( -3.385241169372517955, -79.21212121212087709, -9.605957155564929906 ) ) ;
#6604 = DIRECTION ( 'NONE',  ( -0.000000000000000000, -0.000000000000000000, -1.000000000000000000 ) ) ;
#6605 =( GEOMETRIC_REPRESENTATION_CONTEXT ( 3 ) GLOBAL_UNCERTAINTY_ASSIGNED_CONTEXT ( ( #13351 ) ) GLOBAL_UNIT_ASSIGNED_CONTEXT ( ( #3937, #8082, #6049 ) ) REPRESENTATION_CONTEXT ( 'NONE', 'WORKASPACE' ) );
#6606 = ADVANCED_FACE ( 'NONE', ( #10116 ), #4111, .T. ) ;
#6607 = DIRECTION ( 'NONE',  ( -0.000000000000000000, -0.000000000000000000, -1.000000000000000000 ) ) ;
#6608 = ADVANCED_FACE ( 'NONE', ( #11089 ), #8921, .F. ) ;
#6609 = ORIENTED_EDGE ( 'NONE', *, *, #2502, .T. ) ;
#6610 = LINE ( 'NONE', #10944, #7199 ) ;
#6611 = DIRECTION ( 'NONE',  ( -6.158143864569485777E-17, -2.736152283717910599E-16, 1.000000000000000000 ) ) ;
#6612 = EDGE_LOOP ( 'NONE', ( #2308, #177, #3745, #1422 ) ) ;
#6613 = CIRCLE ( 'NONE', #5050, 25.50000000002549783 ) ;
#6614 = CYLINDRICAL_SURFACE ( 'NONE', #9522, 9.000000000008999024 ) ;
#6615 = CYLINDRICAL_SURFACE ( 'NONE', #3828, 14.99999999999999645 ) ;
#6616 = ORIENTED_EDGE ( 'NONE', *, *, #12552, .T. ) ;
#6617 = CARTESIAN_POINT ( 'NONE',  ( 35.00000000000001421, -34.99999999999999289, 7.500000000000000000 ) ) ;
#6618 = ORIENTED_EDGE ( 'NONE', *, *, #8007, .T. ) ;
#6619 = CARTESIAN_POINT ( 'NONE',  ( -1.219787497442949287E-15, 43.60378069071538221, -7.699803463976802609E-17 ) ) ;
#6620 = FACE_OUTER_BOUND ( 'NONE', #732, .T. ) ;
#6621 = EDGE_CURVE ( 'NONE', #6312, #10695, #5939, .T. ) ;
#6622 = CARTESIAN_POINT ( 'NONE',  ( 34.91511737228310608, 106.7798435036222884, -2.458454180825599078 ) ) ;
#6623 =( BOUNDED_SURFACE ( )  B_SPLINE_SURFACE ( 3, 3, ( 
 ( #9391, #2868, #11352, #2016 ),
 ( #5105, #12691, #974, #3068 ),
 ( #7142, #11419, #3982, #9521 ),
 ( #6233, #10571, #6031, #11559 ) ),
 .UNSPECIFIED., .F., .F., .T. ) 
 B_SPLINE_SURFACE_WITH_KNOTS ( ( 4, 4 ),
 ( 4, 4 ),
 ( 0.000000000000000000, 1.000000000000000000 ),
 ( 0.000000000000000000, 1.000000000000000000 ),
 .UNSPECIFIED. ) 
 GEOMETRIC_REPRESENTATION_ITEM ( )  RATIONAL_B_SPLINE_SURFACE ( (
 ( 1.000000000000000000, 0.3333333333333334259, 0.3333333333333334259, 1.000000000000000000),
 ( 1.000000000000000000, 0.3333333333333334259, 0.3333333333333334259, 1.000000000000000000),
 ( 1.000000000000000000, 0.3333333333333334259, 0.3333333333333334259, 1.000000000000000000),
 ( 1.000000000000000000, 0.3333333333333334259, 0.3333333333333334259, 1.000000000000000000) ) ) 
 REPRESENTATION_ITEM ( '' )  SURFACE ( )  );
#6624 = CARTESIAN_POINT ( 'NONE',  ( 15.29705854078138749, 90.00000000000000000, 1.714422261702872371E-15 ) ) ;
#6625 = DIRECTION ( 'NONE',  ( 1.000000000000000000, -8.163404592832038896E-16, 0.000000000000000000 ) ) ;
#6626 = CARTESIAN_POINT ( 'NONE',  ( -12.99579180576517423, -30.16426982310158067, -1.484993918994249462E-15 ) ) ;
#6627 = AXIS2_PLACEMENT_3D ( 'NONE', #11424, #9580, #3193 ) ;
#6628 = EDGE_CURVE ( 'NONE', #6322, #6577, #525, .T. ) ;
#6629 = CARTESIAN_POINT ( 'NONE',  ( -2.517691654963332357E-15, 90.00000000000000000, -1.589271161308885878E-16 ) ) ;
#6630 = CARTESIAN_POINT ( 'NONE',  ( 12.99579180576516357, 16.95961992694555676, 3.183050967463141802E-15 ) ) ;
#6631 = CARTESIAN_POINT ( 'NONE',  ( 30.45476892764376231, 18.18971895053902443, -2.499999999999993783 ) ) ;
#6632 = ORIENTED_EDGE ( 'NONE', *, *, #3340, .T. ) ;
#6633 = DIRECTION ( 'NONE',  ( -0.000000000000000000, -0.000000000000000000, -1.000000000000000000 ) ) ;
#6634 = ORIENTED_EDGE ( 'NONE', *, *, #560, .T. ) ;
#6635 = CYLINDRICAL_SURFACE ( 'NONE', #10176, 9.000000000008999024 ) ;
#6636 = PRODUCT_CONTEXT ( 'NONE', #5047, 'mechanical' ) ;
#6637 = ORIENTED_EDGE ( 'NONE', *, *, #6216, .F. ) ;
#6638 = CARTESIAN_POINT ( 'NONE',  ( -31.81818181818181657, 133.3608531424536920, 2.500000000000000000 ) ) ;
#6639 = CARTESIAN_POINT ( 'NONE',  ( -10.69381717166375800, 53.83378072214353693, -1.499740397452121781E-15 ) ) ;
#6640 = LINE ( 'NONE', #10981, #3639 ) ;
#6641 = AXIS2_PLACEMENT_3D ( 'NONE', #6160, #832, #2076 ) ;
#6642 = DIRECTION ( 'NONE',  ( -0.000000000000000000, -0.000000000000000000, -1.000000000000000000 ) ) ;
#6643 = ORIENTED_EDGE ( 'NONE', *, *, #6360, .T. ) ;
#6644 = EDGE_CURVE ( 'NONE', #8513, #4067, #11963, .T. ) ;
#6645 = ORIENTED_EDGE ( 'NONE', *, *, #9518, .T. ) ;
#6646 = AXIS2_PLACEMENT_3D ( 'NONE', #10000, #410, #4663 ) ;
#6647 = ORIENTED_EDGE ( 'NONE', *, *, #9619, .T. ) ;
#6648 = FACE_OUTER_BOUND ( 'NONE', #7117, .T. ) ;
#6649 = ORIENTED_EDGE ( 'NONE', *, *, #6098, .F. ) ;
#6650 = CARTESIAN_POINT ( 'NONE',  ( -8.385254915620292238, 71.87811454074363837, -1.280750480509034654E-15 ) ) ;
#6651 = DIRECTION ( 'NONE',  ( -6.158143864569485777E-17, -2.736152283717910599E-16, 1.000000000000000000 ) ) ;
#6652 = CARTESIAN_POINT ( 'NONE',  ( 15.18222645069203125, 20.00000000000000355, 4.000000000000000000 ) ) ;
#6653 = DIRECTION ( 'NONE',  ( 1.000000000000000000, 0.000000000000000000, 0.000000000000000000 ) ) ;
#6654 = CARTESIAN_POINT ( 'NONE',  ( 2.766098618134335663, 90.01525736159537416, -4.178197917109232051 ) ) ;
#6655 = CARTESIAN_POINT ( 'NONE',  ( -7.746655750637584603, -88.96548976718894153, 4.603499224255631184 ) ) ;
#6656 = DIRECTION ( 'NONE',  ( -6.158143864569485777E-17, -2.736152283717910599E-16, 1.000000000000000000 ) ) ;
#6657 = ORIENTED_EDGE ( 'NONE', *, *, #8834, .T. ) ;
#6658 = ORIENTED_EDGE ( 'NONE', *, *, #1654, .T. ) ;
#6659 = EDGE_CURVE ( 'NONE', #6312, #10078, #8013, .T. ) ;
#6660 = CARTESIAN_POINT ( 'NONE',  ( -4.066030946031339077, 90.77438413795603367, 2.912544222229247470 ) ) ;
#6661 = DIRECTION ( 'NONE',  ( 0.000000000000000000, 0.000000000000000000, 1.000000000000000000 ) ) ;
#6662 = VERTEX_POINT ( 'NONE', #6102 ) ;
#6663 = CARTESIAN_POINT ( 'NONE',  ( -12.99579180576517068, 35.80917582696438473, 25.99158361153032359 ) ) ;
#6664 = CARTESIAN_POINT ( 'NONE',  ( 15.29705854078139282, 8.361467971976955127, -30.59411708156277498 ) ) ;
#6665 = DIRECTION ( 'NONE',  ( 0.9960067511297463483, -0.08927794634716618161, 4.818676322152979407E-17 ) ) ;
#6666 = CARTESIAN_POINT ( 'NONE',  ( -32.50000000000000000, -3.980102097228898626E-15, -7.500000000000000000 ) ) ;
#6667 = CARTESIAN_POINT ( 'NONE',  ( 10.69381717166375445, 44.40900277213413716, 0.000000000000000000 ) ) ;
#6668 = DIRECTION ( 'NONE',  ( -0.4545454545454558626, 0.8907235428302457958, 0.000000000000000000 ) ) ;
#6669 = CARTESIAN_POINT ( 'NONE',  ( 23.90723890023449627, -15.11541108221136476, 2.499999999999995115 ) ) ;
#6670 = CIRCLE ( 'NONE', #2880, 10.00000000000000178 ) ;
#6671 = ORIENTED_EDGE ( 'NONE', *, *, #13131, .F. ) ;
#6672 = ORIENTED_EDGE ( 'NONE', *, *, #1809, .F. ) ;
#6673 = VECTOR ( 'NONE', #9885, 1000.000000000000000 ) ;
#6674 = EDGE_CURVE ( 'NONE', #12816, #2145, #7267, .T. ) ;
#6675 = DIRECTION ( 'NONE',  ( 0.000000000000000000, 1.000000000000000000, -0.000000000000000000 ) ) ;
#6676 = ORIENTED_EDGE ( 'NONE', *, *, #5736, .T. ) ;
#6677 = EDGE_CURVE ( 'NONE', #3661, #425, #3911, .T. ) ;
#6678 = FACE_OUTER_BOUND ( 'NONE', #5102, .T. ) ;
#6679 = FACE_OUTER_BOUND ( 'NONE', #12268, .T. ) ;
#6680 = DIRECTION ( 'NONE',  ( -0.000000000000000000, -0.000000000000000000, -1.000000000000000000 ) ) ;
#6681 = ADVANCED_FACE ( 'NONE', ( #9524 ), #1449, .T. ) ;
#6682 = VERTEX_POINT ( 'NONE', #10501 ) ;
#6683 = ORIENTED_EDGE ( 'NONE', *, *, #3318, .T. ) ;
#6684 = CARTESIAN_POINT ( 'NONE',  ( -15.29705854078139105, 8.361467971976981772, -1.476515546007874940E-17 ) ) ;
#6685 = EDGE_CURVE ( 'NONE', #6758, #5520, #2085, .T. ) ;
#6686 = CARTESIAN_POINT ( 'NONE',  ( -8.385254915620292238, 71.87811454074363837, -1.269264606320675724E-16 ) ) ;
#6687 = AXIS2_PLACEMENT_3D ( 'NONE', #10761, #11685, #12960 ) ;
#6688 = FACE_OUTER_BOUND ( 'NONE', #3994, .T. ) ;
#6689 = CARTESIAN_POINT ( 'NONE',  ( -10.69381717166375623, 44.40900277213413716, -2.718044847157924077E-15 ) ) ;
#6690 = CARTESIAN_POINT ( 'NONE',  ( 35.06230589874905235, 106.5835921350012967, -2.486789939184903986 ) ) ;
#6691 = DIRECTION ( 'NONE',  ( -1.000000000000000000, 0.000000000000000000, 0.000000000000000000 ) ) ;
#6692 = CARTESIAN_POINT ( 'NONE',  ( -39.42607625790187598, 101.2633694847512800, -2.396914520158672790 ) ) ;
#6693 = CARTESIAN_POINT ( 'NONE',  ( 40.79557129359545797, 100.6404192164768716, 0.7730400384045159612 ) ) ;
#6694 = DIRECTION ( 'NONE',  ( -1.000000000000000000, 0.000000000000000000, 0.000000000000000000 ) ) ;
#6695 = FACE_OUTER_BOUND ( 'NONE', #9351, .T. ) ;
#6696 = VERTEX_POINT ( 'NONE', #903 ) ;
#6697 = CIRCLE ( 'NONE', #8050, 25.50000000002549783 ) ;
#6698 = VERTEX_POINT ( 'NONE', #840 ) ;
#6699 = DIRECTION ( 'NONE',  ( 0.000000000000000000, 1.000000000000000000, 0.000000000000000000 ) ) ;
#6700 = CIRCLE ( 'NONE', #4689, 2.000000000000000000 ) ;
#6701 = EDGE_CURVE ( 'NONE', #9123, #3490, #4181, .T. ) ;
#6702 = ORIENTED_EDGE ( 'NONE', *, *, #12808, .F. ) ;
#6703 = EDGE_CURVE ( 'NONE', #7522, #3490, #13803, .T. ) ;
#6704 = CARTESIAN_POINT ( 'NONE',  ( 10.69346802281034670, 49.59884612375012125, 0.000000000000000000 ) ) ;
#6705 = ORIENTED_EDGE ( 'NONE', *, *, #8673, .F. ) ;
#6706 = DIRECTION ( 'NONE',  ( 0.4545454545454548634, 0.8907235428302464619, 0.000000000000000000 ) ) ;
#6707 = CIRCLE ( 'NONE', #5362, 5.000000000000000000 ) ;
#6708 = EDGE_CURVE ( 'NONE', #10788, #11146, #11495, .T. ) ;
#6709 = CARTESIAN_POINT ( 'NONE',  ( 25.00000000000000355, 120.0000000000000284, -2.500000000000000000 ) ) ;
#6710 = CIRCLE ( 'NONE', #9417, 10.00000000000000178 ) ;
#6711 = CARTESIAN_POINT ( 'NONE',  ( 24.37649275748779232, -100.0000000000000000, 7.500000000000000000 ) ) ;
#6712 = VECTOR ( 'NONE', #3309, 1000.000000000000000 ) ;
#6713 = DIRECTION ( 'NONE',  ( 1.000000000000000000, 0.000000000000000000, 0.000000000000000000 ) ) ;
#6714 = ORIENTED_EDGE ( 'NONE', *, *, #2669, .F. ) ;
#6715 = ORIENTED_EDGE ( 'NONE', *, *, #10567, .T. ) ;
#6716 = VERTEX_POINT ( 'NONE', #13708 ) ;
#6717 = AXIS2_PLACEMENT_3D ( 'NONE', #13727, #6193, #4992 ) ;
#6718 = LINE ( 'NONE', #5590, #6076 ) ;
#6719 = EDGE_CURVE ( 'NONE', #13844, #973, #5239, .T. ) ;
#6720 = AXIS2_PLACEMENT_3D ( 'NONE', #12405, #12472, #2855 ) ;
#6721 = CIRCLE ( 'NONE', #5592, 10.00000000000000178 ) ;
#6722 = VERTEX_POINT ( 'NONE', #3004 ) ;
#6723 = CARTESIAN_POINT ( 'NONE',  ( -35.00000000000000000, -4.286263797015736496E-15, -7.500000000000000000 ) ) ;
#6724 = CARTESIAN_POINT ( 'NONE',  ( 19.02348910326480436, 26.95332645987221909, -6.306009631028899776 ) ) ;
#6725 = DIRECTION ( 'NONE',  ( 0.000000000000000000, 0.000000000000000000, 1.000000000000000000 ) ) ;
#6726 = CARTESIAN_POINT ( 'NONE',  ( 48.00000000000000000, 120.0000000000000142, -2.500000000000000000 ) ) ;
#6727 = CIRCLE ( 'NONE', #29, 2.000000000000003997 ) ;
#6728 = CARTESIAN_POINT ( 'NONE',  ( -8.308237197123997220, -90.29822314243337189, 3.067701055007814759 ) ) ;
#6729 = ORIENTED_EDGE ( 'NONE', *, *, #7040, .T. ) ;
#6730 = AXIS2_PLACEMENT_3D ( 'NONE', #1128, #10845, #10777 ) ;
#6731 = AXIS2_PLACEMENT_3D ( 'NONE', #3398, #1300, #8960 ) ;
#6732 = EDGE_LOOP ( 'NONE', ( #5990, #7051, #285, #8116, #487, #1936 ) ) ;
#6733 = VERTEX_POINT ( 'NONE', #3202 ) ;
#6734 = ORIENTED_EDGE ( 'NONE', *, *, #12370, .T. ) ;
#6735 = DIRECTION ( 'NONE',  ( 1.000000000000000000, 1.224646799147353207E-16, 0.000000000000000000 ) ) ;
#6736 = ORIENTED_EDGE ( 'NONE', *, *, #12391, .F. ) ;
#6737 = CARTESIAN_POINT ( 'NONE',  ( -8.385254915620294014, -3.520109059331755663, 16.77050983124058092 ) ) ;
#6738 =( NAMED_UNIT ( * ) PLANE_ANGLE_UNIT ( ) SI_UNIT ( $, .RADIAN. ) );
#6739 = CARTESIAN_POINT ( 'NONE',  ( -10.69346802281034670, 59.02362407375952102, -2.757941663132658262E-15 ) ) ;
#6740 = AXIS2_PLACEMENT_3D ( 'NONE', #7843, #3632, #13206 ) ;
#6741 = DIRECTION ( 'NONE',  ( -0.000000000000000000, -0.000000000000000000, -1.000000000000000000 ) ) ;
#6742 = CIRCLE ( 'NONE', #5173, 14.99999999999999112 ) ;
#6743 = CARTESIAN_POINT ( 'NONE',  ( 3.341303593453228693, -106.9090909090940187, -6.231874970757119492 ) ) ;
#6744 = CARTESIAN_POINT ( 'NONE',  ( 10.00000000000000000, 90.00000000000000000, -0.5000000000000000000 ) ) ;
#6745 = DIRECTION ( 'NONE',  ( 1.000000000000000000, 0.000000000000000000, 0.000000000000000000 ) ) ;
#6746 = FACE_OUTER_BOUND ( 'NONE', #3777, .T. ) ;
#6747 = DIRECTION ( 'NONE',  ( 0.9960067511297463483, -0.08927794634716618161, 4.818676322152979407E-17 ) ) ;
#6748 = CARTESIAN_POINT ( 'NONE',  ( -8.385254915620292238, 34.17900274070598243, -6.035522597566817733E-17 ) ) ;
#6749 = DIRECTION ( 'NONE',  ( 0.000000000000000000, 0.000000000000000000, 1.000000000000000000 ) ) ;
#6750 = ORIENTED_EDGE ( 'NONE', *, *, #2223, .T. ) ;
#6751 = ORIENTED_EDGE ( 'NONE', *, *, #10419, .T. ) ;
#6752 = VERTEX_POINT ( 'NONE', #2215 ) ;
#6753 = CIRCLE ( 'NONE', #9452, 25.50000000002549783 ) ;
#6754 = DIRECTION ( 'NONE',  ( 0.000000000000000000, 0.000000000000000000, 1.000000000000000000 ) ) ;
#6755 = LINE ( 'NONE', #11023, #7607 ) ;
#6756 = DIRECTION ( 'NONE',  ( -1.000000000000000000, 0.000000000000000000, 0.000000000000000000 ) ) ;
#6757 = ORIENTED_EDGE ( 'NONE', *, *, #12611, .F. ) ;
#6758 = VERTEX_POINT ( 'NONE', #13771 ) ;
#6759 = LINE ( 'NONE', #12088, #13117 ) ;
#6760 = DIRECTION ( 'NONE',  ( -6.158143864569485777E-17, -2.736152283717910599E-16, 1.000000000000000000 ) ) ;
#6761 = CARTESIAN_POINT ( 'NONE',  ( 4.696430422119469483, 90.40949893945196436, -1.719416569030751685 ) ) ;
#6762 = CARTESIAN_POINT ( 'NONE',  ( 15.29705854078138749, 17.78624592198638155, 1.840275709580739737E-15 ) ) ;
#6763 = CARTESIAN_POINT ( 'NONE',  ( 34.37544226909922429, 107.8407100838017385, -1.642507177281958830 ) ) ;
#6764 = PRODUCT_DEFINITION_SHAPE ( 'NONE', 'NONE',  #9678 ) ;
#6765 = EDGE_CURVE ( 'NONE', #9535, #10692, #65, .T. ) ;
#6766 = DIRECTION ( 'NONE',  ( 1.000000000000000000, 0.000000000000000000, 0.000000000000000000 ) ) ;
#6767 = DIRECTION ( 'NONE',  ( -0.1234677578012386562, -1.701584941912606716E-18, 0.9923485843107423543 ) ) ;
#6768 = PRESENTATION_STYLE_ASSIGNMENT (( #1112 ) ) ;
#6769 = ADVANCED_FACE ( 'NONE', ( #8536 ), #4250, .T. ) ;
#6770 = DIRECTION ( 'NONE',  ( 0.9960067511297463483, -0.08927794634716620936, 4.626175998653454121E-17 ) ) ;
#6771 = FACE_OUTER_BOUND ( 'NONE', #3814, .T. ) ;
#6772 = DIRECTION ( 'NONE',  ( -0.3926913852462016186, -0.9196703082917373484, -2.891205793291787644E-16 ) ) ;
#6773 = CARTESIAN_POINT ( 'NONE',  ( 3.828914887500465269, 90.45818551217382719, 3.218881588266133686 ) ) ;
#6774 = ORIENTED_EDGE ( 'NONE', *, *, #9671, .T. ) ;
#6775 = CARTESIAN_POINT ( 'NONE',  ( -15.29705854078139105, 47.94714734142005597, -8.466779837416320124E-17 ) ) ;
#6776 = VERTEX_POINT ( 'NONE', #2017 ) ;
#6777 = DIRECTION ( 'NONE',  ( -2.797435172181481150E-17, 1.000000000000000000, -1.765856845898762549E-18 ) ) ;
#6778 =( NAMED_UNIT ( * ) SI_UNIT ( $, .STERADIAN. ) SOLID_ANGLE_UNIT ( ) );
#6779 = VERTEX_POINT ( 'NONE', #6302 ) ;
#6780 = DIRECTION ( 'NONE',  ( 0.000000000000000000, 0.000000000000000000, 1.000000000000000000 ) ) ;
#6781 = EDGE_CURVE ( 'NONE', #4883, #369, #5031, .T. ) ;
#6782 = CIRCLE ( 'NONE', #11488, 15.29705854078139460 ) ;
#6783 = CARTESIAN_POINT ( 'NONE',  ( 25.00000000000000711, -34.99999999999999289, 7.500000000000000000 ) ) ;
#6784 = AXIS2_PLACEMENT_3D ( 'NONE', #1147, #5687, #7575 ) ;
#6785 = DIRECTION ( 'NONE',  ( -0.000000000000000000, -0.000000000000000000, -1.000000000000000000 ) ) ;
#6786 = CARTESIAN_POINT ( 'NONE',  ( 10.07809618175545552, -70.83793457269361227, 0.9291402596207405384 ) ) ;
#6787 = EDGE_CURVE ( 'NONE', #624, #3971, #9288, .T. ) ;
#6788 = ORIENTED_EDGE ( 'NONE', *, *, #10887, .T. ) ;
#6789 = EDGE_CURVE ( 'NONE', #2423, #5794, #8600, .T. ) ;
#6790 = AXIS2_PLACEMENT_3D ( 'NONE', #6537, #231, #13077 ) ;
#6791 = DIRECTION ( 'NONE',  ( 0.000000000000000000, -0.000000000000000000, -1.000000000000000000 ) ) ;
#6792 = VERTEX_POINT ( 'NONE', #203 ) ;
#6793 = DIRECTION ( 'NONE',  ( 1.000000000000000000, 0.000000000000000000, 0.000000000000000000 ) ) ;
#6794 = ORIENTED_EDGE ( 'NONE', *, *, #6644, .T. ) ;
#6795 = VERTEX_POINT ( 'NONE', #4678 ) ;
#6796 = PRESENTATION_STYLE_ASSIGNMENT (( #2519 ) ) ;
#6797 = CARTESIAN_POINT ( 'NONE',  ( -31.93204061526060045, -3.910547132972217398E-15, 0.000000000000000000 ) ) ;
#6798 = EDGE_CURVE ( 'NONE', #9003, #10135, #9798, .T. ) ;
#6799 = PRESENTATION_LAYER_ASSIGNMENT (  '', '', ( #5015 ) ) ;
#6800 = LINE ( 'NONE', #510, #8068 ) ;
#6801 = CARTESIAN_POINT ( 'NONE',  ( 25.00000000000000355, 120.0000000000000142, 2.499999999999999556 ) ) ;
#6802 = CARTESIAN_POINT ( 'NONE',  ( 15.29705854078138927, 66.79670324143890525, -30.59411708156276788 ) ) ;
#6803 = CARTESIAN_POINT ( 'NONE',  ( -8.385254915620294014, -31.79444290936001138, -1.999968028543267754E-15 ) ) ;
#6804 = EDGE_CURVE ( 'NONE', #1659, #4720, #12114, .T. ) ;
#6805 = ORIENTED_EDGE ( 'NONE', *, *, #3842, .F. ) ;
#6806 = AXIS2_PLACEMENT_3D ( 'NONE', #1667, #5882, #10223 ) ;
#6807 = ORIENTED_EDGE ( 'NONE', *, *, #10710, .T. ) ;
#6808 = FACE_OUTER_BOUND ( 'NONE', #9540, .T. ) ;
#6809 = CARTESIAN_POINT ( 'NONE',  ( -0.2617580721752758022, -80.12121212121192571, 10.03731802028323727 ) ) ;
#6810 = VERTEX_POINT ( 'NONE', #13272 ) ;
#6811 = CARTESIAN_POINT ( 'NONE',  ( -60.00000000000001421, 20.00000000000000000, -4.000000000000000000 ) ) ;
#6812 =( LENGTH_UNIT ( ) NAMED_UNIT ( * ) SI_UNIT ( .MILLI., .METRE. ) );
#6813 = DIRECTION ( 'NONE',  ( 0.000000000000000000, 0.000000000000000000, -1.000000000000000000 ) ) ;
#6814 = CARTESIAN_POINT ( 'NONE',  ( 34.99999999999958789, 1.104930248025249758E-13, -2.499999999999999112 ) ) ;
#6815 = CARTESIAN_POINT ( 'NONE',  ( 40.87368016229836343, -22.78235879061915270, -2.500000000000000000 ) ) ;
#6816 = CARTESIAN_POINT ( 'NONE',  ( 10.69346802281035202, -16.37459952631584059, -21.38693604562069339 ) ) ;
#6817 = CARTESIAN_POINT ( 'NONE',  ( 6.635975953253233861, -85.78354978353411298, -7.919939413331956501 ) ) ;
#6818 = DIRECTION ( 'NONE',  ( -0.000000000000000000, -0.000000000000000000, -1.000000000000000000 ) ) ;
#6819 = CARTESIAN_POINT ( 'NONE',  ( 19.06870874253413461, 13.90050210118286245, -2.499999999999996447 ) ) ;
#6820 = DIRECTION ( 'NONE',  ( -6.158143864569485777E-17, -2.736152283717910599E-16, 1.000000000000000000 ) ) ;
#6821 = VECTOR ( 'NONE', #8119, 1000.000000000000000 ) ;
#6822 = EDGE_LOOP ( 'NONE', ( #13359, #9339, #12253, #13530, #1092, #5418 ) ) ;
#6823 = ORIENTED_EDGE ( 'NONE', *, *, #8070, .T. ) ;
#6824 = EDGE_LOOP ( 'NONE', ( #4395, #9407, #200, #3443 ) ) ;
#6825 = CARTESIAN_POINT ( 'NONE',  ( -32.50000000000000000, -3.980102097228898626E-15, 7.500000000000000000 ) ) ;
#6826 = CIRCLE ( 'NONE', #6166, 8.385254915620292238 ) ;
#6827 = ORIENTED_EDGE ( 'NONE', *, *, #11484, .T. ) ;
#6828 = CARTESIAN_POINT ( 'NONE',  ( -1.339511369751129832, -125.0784420352225368, 4.454679473787292565 ) ) ;
#6829 = DIRECTION ( 'NONE',  ( -0.000000000000000000, 0.000000000000000000, -1.000000000000000000 ) ) ;
#6830 = CARTESIAN_POINT ( 'NONE',  ( -18.54049621773915746, -20.00000000000000000, -7.500000000000000000 ) ) ;
#6831 = CARTESIAN_POINT ( 'NONE',  ( 19.18070798040252356, 20.00000000000000000, -4.000000000000000000 ) ) ;
#6832 = ORIENTED_EDGE ( 'NONE', *, *, #3408, .T. ) ;
#6834 = ORIENTED_EDGE ( 'NONE', *, *, #9279, .T. ) ;
#6833 = AXIS2_PLACEMENT_3D ( 'NONE', #7577, #8631, #4414 ) ;
#6835 = LINE ( 'NONE', #11877, #4584 ) ;
#6836 = ORIENTED_EDGE ( 'NONE', *, *, #12173, .T. ) ;
#6837 = CARTESIAN_POINT ( 'NONE',  ( 32.72727272727274084, 135.1423002281142089, 2.500000000000000000 ) ) ;
#6838 = DIRECTION ( 'NONE',  ( 1.000000000000000000, 0.000000000000000000, 0.000000000000000000 ) ) ;
#6839 = CIRCLE ( 'NONE', #132, 80.00000000000001421 ) ;
#6840 = DIRECTION ( 'NONE',  ( 0.000000000000000000, -0.000000000000000000, 1.000000000000000000 ) ) ;
#6841 = CARTESIAN_POINT ( 'NONE',  ( -10.69346802281034847, 68.44840202376897764, -1.551312297200932909E-15 ) ) ;
#6842 =( NAMED_UNIT ( * ) PLANE_ANGLE_UNIT ( ) SI_UNIT ( $, .RADIAN. ) );
#6843 = CYLINDRICAL_SURFACE ( 'NONE', #12863, 12.49999999999999112 ) ;
#6844 = DIRECTION ( 'NONE',  ( -1.000000000000000000, 0.000000000000000000, 0.000000000000000000 ) ) ;
#6845 = CARTESIAN_POINT ( 'NONE',  ( 12.99553232110414491, -7.774801155466914970, 1.605812573171299022E-15 ) ) ;
#6846 = CIRCLE ( 'NONE', #5486, 9.000000000009002576 ) ;
#6847 = ORIENTED_EDGE ( 'NONE', *, *, #9699, .T. ) ;
#6848 = CIRCLE ( 'NONE', #2591, 12.49999999999998757 ) ;
#6849 = CARTESIAN_POINT ( 'NONE',  ( 3.784192700541063825, -168.9999999999998010, 1.982393907671174960 ) ) ;
#6850 = CIRCLE ( 'NONE', #598, 10.00000000000000178 ) ;
#6851 = EDGE_CURVE ( 'NONE', #11572, #3347, #4338, .T. ) ;
#6852 = ORIENTED_EDGE ( 'NONE', *, *, #8185, .T. ) ;
#6853 = CARTESIAN_POINT ( 'NONE',  ( 12.99553232110413958, 48.77386654458962312, 0.000000000000000000 ) ) ;
#6854 = VERTEX_POINT ( 'NONE', #2507 ) ;
#6855 = AXIS2_PLACEMENT_3D ( 'NONE', #6386, #2168, #8551 ) ;
#6856 = CARTESIAN_POINT ( 'NONE',  ( -15.29705854078138749, 36.63580182200524149, -30.59411708156277854 ) ) ;
#6857 = DIRECTION ( 'NONE',  ( -0.000000000000000000, -0.000000000000000000, -1.000000000000000000 ) ) ;
#6858 = CARTESIAN_POINT ( 'NONE',  ( 25.00000000000001776, -100.0000000000000000, -7.500000000000000000 ) ) ;
#6859 = CIRCLE ( 'NONE', #11115, 5.000000000000001776 ) ;
#6860 = CARTESIAN_POINT ( 'NONE',  ( -12.99553232110414314, 20.49953269456136695, -1.663892186318449368E-15 ) ) ;
#6861 = UNCERTAINTY_MEASURE_WITH_UNIT (LENGTH_MEASURE( 1.000000000000000082E-05 ), #155, 'distance_accuracy_value', 'NONE');
#6862 = CARTESIAN_POINT ( 'NONE',  ( -15.29705854078139282, -38.76242177807012723, 30.59411708156277854 ) ) ;
#6863 = ORIENTED_EDGE ( 'NONE', *, *, #6341, .T. ) ;
#6864 = EDGE_LOOP ( 'NONE', ( #13367, #3721, #3493, #9085 ) ) ;
#6865 = EDGE_CURVE ( 'NONE', #7675, #780, #574, .T. ) ;
#6866 = CARTESIAN_POINT ( 'NONE',  ( -15.29705854078138927, -27.45107625865536960, -30.59411708156278564 ) ) ;
#6867 = EDGE_CURVE ( 'NONE', #11197, #6577, #111, .T. ) ;
#6868 = ORIENTED_EDGE ( 'NONE', *, *, #1809, .T. ) ;
#6869 = ORIENTED_EDGE ( 'NONE', *, *, #6899, .F. ) ;
#6870 = EDGE_CURVE ( 'NONE', #8621, #2743, #1894, .T. ) ;
#6871 = DIRECTION ( 'NONE',  ( 2.797435172181480534E-17, -1.000000000000000000, 1.765856845898762164E-18 ) ) ;
#6872 = ADVANCED_FACE ( 'NONE', ( #5440 ), #2330, .T. ) ;
#6873 = CIRCLE ( 'NONE', #10235, 11.81226048336476886 ) ;
#6874 = CARTESIAN_POINT ( 'NONE',  ( -10.69346802281035202, 77.87317997377837742, -1.584597914529132607E-15 ) ) ;
#6875 = CARTESIAN_POINT ( 'NONE',  ( -35.00000000000000000, -4.286263797015736496E-15, 7.500000000000000000 ) ) ;
#6876 = CARTESIAN_POINT ( 'NONE',  ( -34.33120614476065668, 107.9646345552176001, 1.436946644489085267 ) ) ;
#6877 = CARTESIAN_POINT ( 'NONE',  ( 2.209461285238361494, -83.12085171535194661, -9.413399924858527612 ) ) ;
#6878 = VERTEX_POINT ( 'NONE', #138 ) ;
#6879 = ORIENTED_EDGE ( 'NONE', *, *, #4359, .F. ) ;
#6880 = ORIENTED_EDGE ( 'NONE', *, *, #8589, .F. ) ;
#6881 = CARTESIAN_POINT ( 'NONE',  ( 0.000000000000000000, 71.01020514433645303, -2.499999999999998668 ) ) ;
#6882 = CARTESIAN_POINT ( 'NONE',  ( -2.680497156732949637, -80.99999999999998579, 9.800765866881983257 ) ) ;
#6883 = ORIENTED_EDGE ( 'NONE', *, *, #2653, .F. ) ;
#6884 = CARTESIAN_POINT ( 'NONE',  ( 6.850226906711063712, -73.90543882657019026, 7.468286908571726279 ) ) ;
#6885 = EDGE_CURVE ( 'NONE', #9880, #8180, #11054, .T. ) ;
#6886 = CARTESIAN_POINT ( 'NONE',  ( 43.29712336220986657, 19.44704974301885159, -2.499999999999993783 ) ) ;
#6887 = PLANE ( 'NONE',  #5336 ) ;
#6888 = CARTESIAN_POINT ( 'NONE',  ( -1.174765158626910777, -79.03030303034420001, -10.44010582246512264 ) ) ;
#6889 = CARTESIAN_POINT ( 'NONE',  ( 15.68886946032145957, -16.65327071804363612, 0.6902218057983463551 ) ) ;
#6890 = VERTEX_POINT ( 'NONE', #13112 ) ;
#6891 = LINE ( 'NONE', #6825, #8099 ) ;
#6892 = VERTEX_POINT ( 'NONE', #8670 ) ;
#6893 = CARTESIAN_POINT ( 'NONE',  ( 1.896508640845344207, -103.2776239719436120, -7.000734796588814035 ) ) ;
#6894 = CARTESIAN_POINT ( 'NONE',  ( 38.16244658108818300, 102.4500712252157655, 2.500000000000000000 ) ) ;
#6895 = CARTESIAN_POINT ( 'NONE',  ( -4.975586992323414874E-16, 17.78624592198638155, -3.140796412417860432E-17 ) ) ;
#6896 = CARTESIAN_POINT ( 'NONE',  ( -41.00000000000000000, -4.286263797015736496E-15, -7.500000000000000000 ) ) ;
#6897 = ORIENTED_EDGE ( 'NONE', *, *, #5734, .T. ) ;
#6898 = CARTESIAN_POINT ( 'NONE',  ( -1.759686353460360175, -152.7490567289512171, -0.2786442552020600982 ) ) ;
#6899 = EDGE_CURVE ( 'NONE', #575, #10661, #10186, .T. ) ;
#6900 = CARTESIAN_POINT ( 'NONE',  ( -35.22727272727274794, 140.0412797136805523, 2.499999999999999556 ) ) ;
#6901 = DIRECTION ( 'NONE',  ( -2.797435172181481150E-17, 1.000000000000000000, -1.765856845898762549E-18 ) ) ;
#6902 = AXIS2_PLACEMENT_3D ( 'NONE', #7080, #12419, #13213 ) ;
#6903 = CARTESIAN_POINT ( 'NONE',  ( 0.6173387890061953209, -69.99999999999998579, -4.961742921553712549 ) ) ;
#6904 = FACE_OUTER_BOUND ( 'NONE', #2272, .T. ) ;
#6905 = CARTESIAN_POINT ( 'NONE',  ( 15.29705854078139460, -27.45107625865536605, 1.923489752901240361E-15 ) ) ;
#6906 = AXIS2_PLACEMENT_3D ( 'NONE', #9344, #13654, #7227 ) ;
#6907 = DIRECTION ( 'NONE',  ( 1.000000000000000000, 0.000000000000000000, -1.387778780781446464E-15 ) ) ;
#6908 = VERTEX_POINT ( 'NONE', #4451 ) ;
#6909 = CARTESIAN_POINT ( 'NONE',  ( -24.99999999999998934, -100.0000000000000000, 7.500000000000000000 ) ) ;
#6910 = ORIENTED_EDGE ( 'NONE', *, *, #10380, .T. ) ;
#6911 = CARTESIAN_POINT ( 'NONE',  ( 11.72298137502698623, -169.0000000000001137, 2.970135970081305921 ) ) ;
#6912 = CIRCLE ( 'NONE', #8946, 25.50000000002549783 ) ;
#6913 = VERTEX_POINT ( 'NONE', #2287 ) ;
#6914 = DIRECTION ( 'NONE',  ( 0.000000000000000000, 1.000000000000000000, 0.000000000000000000 ) ) ;
#6915 = CARTESIAN_POINT ( 'NONE',  ( 0.000000000000000000, 0.000000000000000000, 0.000000000000000000 ) ) ;
#6916 = CARTESIAN_POINT ( 'NONE',  ( 10.91573825926023922, -140.5584415584475835, 8.453432789889285814 ) ) ;
#6917 = CARTESIAN_POINT ( 'NONE',  ( 50.00000000000000000, 120.0000000000000284, 0.5000000000000000000 ) ) ;
#6918 = CARTESIAN_POINT ( 'NONE',  ( 15.29705854078139282, -19.91286587805129926, 30.59411708156279630 ) ) ;
#6919 = CARTESIAN_POINT ( 'NONE',  ( 19.50211115783503857, -14.38212227840833179, -2.500000000000004441 ) ) ;
#6920 = EDGE_CURVE ( 'NONE', #10078, #618, #5435, .T. ) ;
#6921 = CARTESIAN_POINT ( 'NONE',  ( -12.97449437267217576, -39.59556244224027211, -1.449077110393148750E-15 ) ) ;
#6922 = ORIENTED_EDGE ( 'NONE', *, *, #3182, .T. ) ;
#6923 = ORIENTED_EDGE ( 'NONE', *, *, #11244, .F. ) ;
#6924 = FACE_OUTER_BOUND ( 'NONE', #13574, .T. ) ;
#6925 = VECTOR ( 'NONE', #4087, 1000.000000000000000 ) ;
#6926 = DIRECTION ( 'NONE',  ( -6.158143864569485777E-17, -2.736152283717910599E-16, 1.000000000000000000 ) ) ;
#6927 = ORIENTED_EDGE ( 'NONE', *, *, #6356, .T. ) ;
#6928 = CARTESIAN_POINT ( 'NONE',  ( -8.385254915620294014, -24.99427717735608212, 4.413631546192547049E-17 ) ) ;
#6929 = AXIS2_PLACEMENT_3D ( 'NONE', #680, #5878, #4819 ) ;
#6930 = FACE_OUTER_BOUND ( 'NONE', #599, .T. ) ;
#6931 = DIRECTION ( 'NONE',  ( 0.000000000000000000, 1.000000000000000000, 0.000000000000000000 ) ) ;
#6932 = DIRECTION ( 'NONE',  ( -0.000000000000000000, -0.000000000000000000, -1.000000000000000000 ) ) ;
#6933 = CARTESIAN_POINT ( 'NONE',  ( -4.832052475181153106, -110.7096548574291575, 4.160198837937846505 ) ) ;
#6934 = CYLINDRICAL_SURFACE ( 'NONE', #12524, 9.000000000008999024 ) ;
#6935 = EDGE_CURVE ( 'NONE', #6241, #13463, #3643, .T. ) ;
#6936 = ORIENTED_EDGE ( 'NONE', *, *, #10643, .F. ) ;
#6937 = AXIS2_PLACEMENT_3D ( 'NONE', #10958, #9714, #10818 ) ;
#6938 = CIRCLE ( 'NONE', #9188, 12.49999999999998757 ) ;
#6939 = ORIENTED_EDGE ( 'NONE', *, *, #6549, .F. ) ;
#6940 = ORIENTED_EDGE ( 'NONE', *, *, #12701, .T. ) ;
#6941 = EDGE_CURVE ( 'NONE', #149, #1460, #12495, .T. ) ;
#6942 = CIRCLE ( 'NONE', #12768, 8.385254915620292238 ) ;
#6943 = ORIENTED_EDGE ( 'NONE', *, *, #573, .F. ) ;
#6944 = CARTESIAN_POINT ( 'NONE',  ( -8.385254915620294014, -24.99427717735608212, -9.386249283210493447E-16 ) ) ;
#6945 = DIRECTION ( 'NONE',  ( -1.000000000000000000, 0.000000000000000000, 0.000000000000000000 ) ) ;
#6946 = ORIENTED_EDGE ( 'NONE', *, *, #5232, .T. ) ;
#6947 = CARTESIAN_POINT ( 'NONE',  ( 4.974937185533097050, 90.00000000000000000, 0.5000000000000000000 ) ) ;
#6948 = SHAPE_REPRESENTATION_RELATIONSHIP ( 'NONE' , 'NONE' ,  #1365, #7406 ) ;
#6949 = DIRECTION ( 'NONE',  ( -0.000000000000000000, -0.000000000000000000, -1.000000000000000000 ) ) ;
#6950 = CIRCLE ( 'NONE', #7398, 25.50000000002549783 ) ;
#6951 = FACE_OUTER_BOUND ( 'NONE', #47, .T. ) ;
#6952 = CARTESIAN_POINT ( 'NONE',  ( -15.29705854078139282, -1.063309978032473291, 1.877653204021102445E-18 ) ) ;
#6953 = CARTESIAN_POINT ( 'NONE',  ( -2.491129965232259824, -148.3982683983499271, 1.520867222960083032 ) ) ;
#6954 = AXIS2_PLACEMENT_3D ( 'NONE', #3390, #2488, #3323 ) ;
#6955 = CARTESIAN_POINT ( 'NONE',  ( 48.00000000000000000, 120.0000000000000284, 2.500000000000000000 ) ) ;
#6956 = EDGE_CURVE ( 'NONE', #3001, #2418, #5926, .T. ) ;
#6957 = AXIS2_PLACEMENT_3D ( 'NONE', #1286, #9706, #2555 ) ;
#6958 = CARTESIAN_POINT ( 'NONE',  ( -28.15981099771517648, -27.70535714287384366, -4.000000000000000000 ) ) ;
#6959 = EDGE_CURVE ( 'NONE', #7666, #849, #1208, .T. ) ;
#6960 = CYLINDRICAL_SURFACE ( 'NONE', #11977, 8.385254915620292238 ) ;
#6961 = ORIENTED_EDGE ( 'NONE', *, *, #10786, .F. ) ;
#6962 = EDGE_LOOP ( 'NONE', ( #3510, #8158, #3788, #3670 ) ) ;
#6963 = ORIENTED_EDGE ( 'NONE', *, *, #12271, .F. ) ;
#6964 = DIRECTION ( 'NONE',  ( -2.797435172181481150E-17, 1.000000000000000000, -1.765856845898762549E-18 ) ) ;
#6965 = EDGE_LOOP ( 'NONE', ( #6714, #7030, #8667, #6658 ) ) ;
#6966 = EDGE_CURVE ( 'NONE', #3876, #4722, #3000, .T. ) ;
#6967 = ADVANCED_FACE ( 'NONE', ( #10977 ), #1378, .T. ) ;
#6968 = CARTESIAN_POINT ( 'NONE',  ( 4.479841886641914961, -106.3258580997496239, -5.265075680640510569 ) ) ;
#6969 = LINE ( 'NONE', #3666, #1327 ) ;
#6970 = CIRCLE ( 'NONE', #9878, 48.00000000000001421 ) ;
#6971 = DIRECTION ( 'NONE',  ( -1.000000000000000000, 0.000000000000000000, 0.000000000000000000 ) ) ;
#6972 = CIRCLE ( 'NONE', #12357, 66.25000000000044054 ) ;
#6973 = CIRCLE ( 'NONE', #930, 25.50000000002549783 ) ;
#6974 = DIRECTION ( 'NONE',  ( 0.9960067511297463483, -0.08927794634716618161, 4.818676322152979407E-17 ) ) ;
#6975 = DIRECTION ( 'NONE',  ( 1.000000000000000000, 0.000000000000000000, 0.000000000000000000 ) ) ;
#6976 = ORIENTED_EDGE ( 'NONE', *, *, #9107, .T. ) ;
#6977 = DIRECTION ( 'NONE',  ( 0.9960067511297464593, -0.08927794634716622324, 3.401418580343279473E-17 ) ) ;
#6978 = CARTESIAN_POINT ( 'NONE',  ( -1.495153876773553492, -154.2876702219585070, -0.7369765331111527429 ) ) ;
#6979 = CARTESIAN_POINT ( 'NONE',  ( 4.545390705139091381, 90.76307318580400363, -2.092381513276356575 ) ) ;
#6980 = CARTESIAN_POINT ( 'NONE',  ( -38.89115197531749857, 101.6687180808697377, 2.500000000000000000 ) ) ;
#6981 = DIRECTION ( 'NONE',  ( -0.9960067511297463483, 0.08927794634716619548, -4.626175998653453504E-17 ) ) ;
#6982 = CARTESIAN_POINT ( 'NONE',  ( 8.385254915620295790, -6.144721277337255927, 1.035430912652129043E-15 ) ) ;
#6983 = CARTESIAN_POINT ( 'NONE',  ( 34.99999999999958789, 1.104930248025249758E-13, -2.499999999999999112 ) ) ;
#6984 = EDGE_CURVE ( 'NONE', #750, #3802, #5027, .T. ) ;
#6985 = DIRECTION ( 'NONE',  ( -0.9923485843107423543, -2.797833471351478217E-17, -0.1234677578012386562 ) ) ;
#6986 = CARTESIAN_POINT ( 'NONE',  ( 10.99999999999999289, 147.0000000000000284, -2.499999999999999556 ) ) ;
#6987 = AXIS2_PLACEMENT_3D ( 'NONE', #9087, #3675, #12521 ) ;
#6988 = EDGE_CURVE ( 'NONE', #11311, #9709, #4802, .T. ) ;
#6989 = ORIENTED_EDGE ( 'NONE', *, *, #12483, .F. ) ;
#6990 = CARTESIAN_POINT ( 'NONE',  ( 10.69381717166375800, 53.83378072214353693, -21.38763434332750890 ) ) ;
#6991 = CARTESIAN_POINT ( 'NONE',  ( 6.139211203634872049, -76.35064935069615899, 12.15884065890582555 ) ) ;
#6992 = ORIENTED_EDGE ( 'NONE', *, *, #3718, .F. ) ;
#6993 = ORIENTED_EDGE ( 'NONE', *, *, #10858, .T. ) ;
#6994 = DIRECTION ( 'NONE',  ( 1.000000000000000000, 0.000000000000000000, 0.000000000000000000 ) ) ;
#6995 = CYLINDRICAL_SURFACE ( 'NONE', #1002, 25.50000000002550138 ) ;
#6996 = DIRECTION ( 'NONE',  ( 6.158143864569485777E-17, 2.736152283717910599E-16, -1.000000000000000000 ) ) ;
#6997 = CARTESIAN_POINT ( 'NONE',  ( -32.72727272727271952, 135.1423002281141805, -0.5000000000000000000 ) ) ;
#6998 = DIRECTION ( 'NONE',  ( 1.000000000000000000, 0.000000000000000000, 0.000000000000000000 ) ) ;
#6999 = CARTESIAN_POINT ( 'NONE',  ( 10.69346802281034314, -35.22415542633469698, 21.38693604562069339 ) ) ;
#7000 = VERTEX_POINT ( 'NONE', #13628 ) ;
#7001 = ORIENTED_EDGE ( 'NONE', *, *, #1724, .F. ) ;
#7002 = ORIENTED_EDGE ( 'NONE', *, *, #13430, .F. ) ;
#7003 = ORIENTED_EDGE ( 'NONE', *, *, #7538, .F. ) ;
#7004 = CARTESIAN_POINT ( 'NONE',  ( -15.29705854078138927, -36.87585420866476227, -3.723114491148376223E-15 ) ) ;
#7005 = CARTESIAN_POINT ( 'NONE',  ( -32.72727272727271952, 135.1423002281141805, 2.500000000000000000 ) ) ;
#7006 = CARTESIAN_POINT ( 'NONE',  ( 34.99999999999958789, 1.104930248025249758E-13, -2.499999999999999112 ) ) ;
#7007 = CARTESIAN_POINT ( 'NONE',  ( 37.50000000000000711, 4.592425496802575156E-15, -7.500000000000000000 ) ) ;
#7008 = CARTESIAN_POINT ( 'NONE',  ( -1.483439550716517611E-15, 53.02855864072483882, -9.364084330386787485E-17 ) ) ;
#7009 = CARTESIAN_POINT ( 'NONE',  ( 7.333588550536464190, -88.25569648369631182, -5.386745576991591733 ) ) ;
#7010 = APPLICATION_CONTEXT ( 'automotive_design' ) ;
#7011 = CARTESIAN_POINT ( 'NONE',  ( -10.69381717166375090, 16.13466892210585257, -21.38763434332751245 ) ) ;
#7012 = ORIENTED_EDGE ( 'NONE', *, *, #8487, .F. ) ;
#7013 = AXIS2_PLACEMENT_3D ( 'NONE', #2358, #10833, #5583 ) ;
#7014 = ORIENTED_EDGE ( 'NONE', *, *, #26, .F. ) ;
#7015 = ORIENTED_EDGE ( 'NONE', *, *, #4063, .F. ) ;
#7016 = ADVANCED_FACE ( 'NONE', ( #1520 ), #11841, .T. ) ;
#7017 = DIRECTION ( 'NONE',  ( 1.000000000000000000, 0.000000000000000000, 0.000000000000000000 ) ) ;
#7018 = AXIS2_PLACEMENT_3D ( 'NONE', #12999, #2251, #5615 ) ;
#7019 = CARTESIAN_POINT ( 'NONE',  ( 10.13852281052238702, -69.87878787878717901, -0.9720347947262335531 ) ) ;
#7020 = ORIENTED_EDGE ( 'NONE', *, *, #5513, .F. ) ;
#7021 = CARTESIAN_POINT ( 'NONE',  ( 9.357262991920059392, -70.83714848844999779, 3.840749680622386641 ) ) ;
#7022 = TOROIDAL_SURFACE ( 'NONE', #11048, 42.00000000000001421, 2.000000000000000000 ) ;
#7023 = CARTESIAN_POINT ( 'NONE',  ( 16.85679715600144135, -10.85606698379831947, -2.500000000000003553 ) ) ;
#7024 = CARTESIAN_POINT ( 'NONE',  ( 3.510313888878266120, -133.0909090909286476, -1.034921094667353270 ) ) ;
#7025 = CARTESIAN_POINT ( 'NONE',  ( 16.53267785980283477, 10.29504797295195750, -2.499999999999997335 ) ) ;
#7026 = CYLINDRICAL_SURFACE ( 'NONE', #4209, 8.385254915620295790 ) ;
#7027 = DIRECTION ( 'NONE',  ( 0.1928999275155752480, 0.9812184353977893014, 2.891205793291787644E-16 ) ) ;
#7028 = VERTEX_POINT ( 'NONE', #1735 ) ;
#7029 = ORIENTED_EDGE ( 'NONE', *, *, #12196, .T. ) ;
#7030 = ORIENTED_EDGE ( 'NONE', *, *, #4440, .F. ) ;
#7031 = DIRECTION ( 'NONE',  ( 1.000000000000000000, 0.000000000000000000, 0.000000000000000000 ) ) ;
#7032 = VERTEX_POINT ( 'NONE', #9241 ) ;
#7033 = AXIS2_PLACEMENT_3D ( 'NONE', #9059, #521, #7017 ) ;
#7034 = CARTESIAN_POINT ( 'NONE',  ( -3.251529939683060366, -129.1726566844749016, 2.555676826061363816 ) ) ;
#7035 = CARTESIAN_POINT ( 'NONE',  ( -35.00000000000000000, -35.00000000000000000, 7.500000000000000000 ) ) ;
#7036 = DIRECTION ( 'NONE',  ( -0.000000000000000000, -0.000000000000000000, -1.000000000000000000 ) ) ;
#7037 = ADVANCED_FACE ( 'NONE', ( #13420 ), #2159, .F. ) ;
#7038 = LINE ( 'NONE', #6830, #8856 ) ;
#7039 = CARTESIAN_POINT ( 'NONE',  ( 25.00000000000000355, 120.0000000000000142, -2.499999999999998668 ) ) ;
#7040 = EDGE_CURVE ( 'NONE', #10943, #1175, #12823, .T. ) ;
#7041 = CARTESIAN_POINT ( 'NONE',  ( 2.376601423472834540, -126.9250422869104540, -3.721977556539412202 ) ) ;
#7042 = DIRECTION ( 'NONE',  ( -6.158143864569485777E-17, -2.736152283717910599E-16, 1.000000000000000000 ) ) ;
#7043 = ADVANCED_FACE ( 'NONE', ( #1096 ), #12954, .T. ) ;
#7044 = CIRCLE ( 'NONE', #3913, 2.000000000000001776 ) ;
#7045 = CARTESIAN_POINT ( 'NONE',  ( 55.99165482216006495, 2.525950835318804266, -2.499999999999997335 ) ) ;
#7046 = ADVANCED_FACE ( 'NONE', ( #7598, #408 ), #7806, .F. ) ;
#7047 = CARTESIAN_POINT ( 'NONE',  ( 10.00000000000000000, 90.00000000000000000, -0.5000000000000000000 ) ) ;
#7048 = DIRECTION ( 'NONE',  ( 0.000000000000000000, 0.000000000000000000, 1.000000000000000000 ) ) ;
#7049 = CARTESIAN_POINT ( 'NONE',  ( -10.69346802281035025, 49.59884612375012125, -1.484741062544533711E-15 ) ) ;
#7050 = ORIENTED_EDGE ( 'NONE', *, *, #9673, .F. ) ;
#7051 = ORIENTED_EDGE ( 'NONE', *, *, #3542, .T. ) ;
#7052 = CARTESIAN_POINT ( 'NONE',  ( 12.02287503512517297, -157.8181818181245433, -0.9430477860670277712 ) ) ;
#7053 = ORIENTED_EDGE ( 'NONE', *, *, #3542, .F. ) ;
#7054 = CIRCLE ( 'NONE', #1014, 8.385254915620292238 ) ;
#7055 = VERTEX_POINT ( 'NONE', #2275 ) ;
#7056 = DIRECTION ( 'NONE',  ( 2.797435172181480534E-17, -1.000000000000000000, 1.765856845898762164E-18 ) ) ;
#7057 = CARTESIAN_POINT ( 'NONE',  ( 10.00000000000000000, 92.00000000000000000, 0.5000000000000000000 ) ) ;
#7058 = CARTESIAN_POINT ( 'NONE',  ( 4.607646589139954507, -134.6363636363662408, 0.3820433400543247759 ) ) ;
#7059 = EDGE_CURVE ( 'NONE', #5379, #10090, #7095, .T. ) ;
#7060 = DIRECTION ( 'NONE',  ( 1.000000000000000000, 0.000000000000000000, 0.000000000000000000 ) ) ;
#7061 = CARTESIAN_POINT ( 'NONE',  ( -38.89115197531749857, 101.6687180808697377, 2.500000000000000000 ) ) ;
#7062 = VECTOR ( 'NONE', #8449, 1000.000000000000000 ) ;
#7063 = CARTESIAN_POINT ( 'NONE',  ( 8.385254915620292238, 22.12961257269105531, 2.053795118489800399E-15 ) ) ;
#7064 = CARTESIAN_POINT ( 'NONE',  ( -37.50000000000000711, -4.286263797015736496E-15, -4.000000000000000000 ) ) ;
#7065 = VECTOR ( 'NONE', #3040, 1000.000000000000000 ) ;
#7066 = AXIS2_PLACEMENT_3D ( 'NONE', #13388, #11098, #4644 ) ;
#7067 = EDGE_LOOP ( 'NONE', ( #2883, #6805, #116, #4718 ) ) ;
#7068 = CARTESIAN_POINT ( 'NONE',  ( -8.872490591736925225, -90.06604609259215977, 0.4070912038452756398 ) ) ;
#7069 = TOROIDAL_SURFACE ( 'NONE', #11985, 22.99999999999999289, 2.000000000000000000 ) ;
#7070 = ORIENTED_EDGE ( 'NONE', *, *, #4063, .T. ) ;
#7071 = CARTESIAN_POINT ( 'NONE',  ( 8.385254915620288685, 43.60378069071538221, 9.522168693316292075E-16 ) ) ;
#7072 = EDGE_LOOP ( 'NONE', ( #13411, #9945, #5550, #10257 ) ) ;
#7073 = DIRECTION ( 'NONE',  ( 1.000000000000000000, 0.000000000000000000, 0.000000000000000000 ) ) ;
#7074 = CIRCLE ( 'NONE', #9295, 24.99999999999998934 ) ;
#7075 = ADVANCED_FACE ( 'NONE', ( #5639 ), #3345, .T. ) ;
#7076 = CARTESIAN_POINT ( 'NONE',  ( -15.29705854078139282, 76.22148119144830503, 30.59411708156276788 ) ) ;
#7077 = CARTESIAN_POINT ( 'NONE',  ( 52.85884796071297131, 5.708463060827147828, 2.500000000000002665 ) ) ;
#7078 = CARTESIAN_POINT ( 'NONE',  ( -35.22727272727274794, 140.0412797136805523, -7.500000000000000000 ) ) ;
#7079 = CARTESIAN_POINT ( 'NONE',  ( -5.469814954756211378, -117.2912297489314710, -0.9484627639890558237 ) ) ;
#7080 = CARTESIAN_POINT ( 'NONE',  ( 34.99999999999958789, 1.104930248025249758E-13, -2.499999999999997335 ) ) ;
#7081 = AXIS2_PLACEMENT_3D ( 'NONE', #4475, #156, #79 ) ;
#7082 = EDGE_LOOP ( 'NONE', ( #12835, #2172, #9476, #5136 ) ) ;
#7083 = ORIENTED_EDGE ( 'NONE', *, *, #776, .F. ) ;
#7084 = ORIENTED_EDGE ( 'NONE', *, *, #2119, .F. ) ;
#7085 = EDGE_LOOP ( 'NONE', ( #6359, #1604 ) ) ;
#7086 = CARTESIAN_POINT ( 'NONE',  ( 25.00000000000000355, 120.0000000000000142, -2.500000000000000000 ) ) ;
#7087 = AXIS2_PLACEMENT_3D ( 'NONE', #6505, #10769, #4454 ) ;
#7088 = CARTESIAN_POINT ( 'NONE',  ( 9.536547895815731479, -71.90909090909467238, 3.228601540706608208 ) ) ;
#7089 = ORIENTED_EDGE ( 'NONE', *, *, #8259, .F. ) ;
#7090 = LINE ( 'NONE', #1479, #8142 ) ;
#7091 = CARTESIAN_POINT ( 'NONE',  ( -0.8583871962692122271, -102.5454545454458355, -7.611802117353696495 ) ) ;
#7092 = CARTESIAN_POINT ( 'NONE',  ( -15.29705854078139105, 76.22148119144830503, -1.345962243664627229E-16 ) ) ;
#7093 = CARTESIAN_POINT ( 'NONE',  ( 75.98647239440286683, -111.6214737678657087, 2.500000000000000000 ) ) ;
#7094 = DIRECTION ( 'NONE',  ( 0.000000000000000000, 0.000000000000000000, 1.000000000000000000 ) ) ;
#7095 = B_SPLINE_CURVE_WITH_KNOTS ( 'NONE', 3,
 ( #3321, #8655, #2487, #2409, #8718, #11035, #3387, #6763, #11881, #8870, #1435, #6558, #13025, #10753, #6622, #6690 ),
 .UNSPECIFIED., .F., .F.,
 ( 4, 2, 2, 2, 2, 2, 2, 4 ),
 ( 1.969947839904427242E-07, 0.0003650593540107671415, 0.0007299217132375439157, 0.001094784072464320690, 0.001459646431691097356, 0.001824508790917874239, 0.002189371150144650904, 0.002919095868598195129 ),
 .UNSPECIFIED. ) ;
#7096 = CARTESIAN_POINT ( 'NONE',  ( 0.1852016367012860043, -160.0000000000003126, -1.488522876466233713 ) ) ;
#7097 = DIRECTION ( 'NONE',  ( -0.8735848310779960046, 0.4866719047884612293, 9.637352644305955116E-17 ) ) ;
#7098 = ORIENTED_EDGE ( 'NONE', *, *, #9361, .T. ) ;
#7099 = ORIENTED_EDGE ( 'NONE', *, *, #8331, .T. ) ;
#7100 = EDGE_CURVE ( 'NONE', #5579, #9616, #11204, .T. ) ;
#7101 = CARTESIAN_POINT ( 'NONE',  ( 1.958204620527036497E-15, -70.00000000000000000, 1.236099792129133461E-16 ) ) ;
#7102 = ORIENTED_EDGE ( 'NONE', *, *, #3141, .F. ) ;
#7103 = CARTESIAN_POINT ( 'NONE',  ( -2.887522863561023723, -136.7361086070154954, -1.558166837788810932 ) ) ;
#7104 = CARTESIAN_POINT ( 'NONE',  ( 6.257768754720297677E-16, -22.36966495935058319, 3.950162600893091522E-17 ) ) ;
#7105 =( BOUNDED_SURFACE ( )  B_SPLINE_SURFACE ( 3, 3, ( 
 ( #4058, #3072, #2946, #3986 ),
 ( #2805, #7278, #842, #8132 ),
 ( #773, #9465, #5108, #11624 ),
 ( #3922, #8269, #13569, #2021 ) ),
 .UNSPECIFIED., .F., .F., .T. ) 
 B_SPLINE_SURFACE_WITH_KNOTS ( ( 4, 4 ),
 ( 4, 4 ),
 ( 0.000000000000000000, 1.000000000000000000 ),
 ( 0.000000000000000000, 1.000000000000000000 ),
 .UNSPECIFIED. ) 
 GEOMETRIC_REPRESENTATION_ITEM ( )  RATIONAL_B_SPLINE_SURFACE ( (
 ( 1.000000000000000000, 0.3333333333333334259, 0.3333333333333334259, 1.000000000000000000),
 ( 1.000000000000000000, 0.3333333333333334259, 0.3333333333333334259, 1.000000000000000000),
 ( 1.000000000000000000, 0.3333333333333334259, 0.3333333333333334259, 1.000000000000000000),
 ( 1.000000000000000000, 0.3333333333333334259, 0.3333333333333334259, 1.000000000000000000) ) ) 
 REPRESENTATION_ITEM ( '' )  SURFACE ( )  );
#7106 = CARTESIAN_POINT ( 'NONE',  ( -32.72727272727271952, 135.1423002281141805, -2.500000000000000000 ) ) ;
#7107 = CARTESIAN_POINT ( 'NONE',  ( 39.08445607832919677, 20.74481184150345214, 2.500000000000006217 ) ) ;
#7108 = DIRECTION ( 'NONE',  ( -2.797435172181481150E-17, 1.000000000000000000, -1.765856845898762549E-18 ) ) ;
#7109 = CARTESIAN_POINT ( 'NONE',  ( -1.659392250802589341, -148.6675893744416896, 1.251955227480716193 ) ) ;
#7110 = PLANE ( 'NONE',  #8756 ) ;
#7111 = LINE ( 'NONE', #8169, #7373 ) ;
#7112 = DIRECTION ( 'NONE',  ( -6.158143864569485777E-17, -2.736152283717910599E-16, 1.000000000000000000 ) ) ;
#7113 = DIRECTION ( 'NONE',  ( -2.797435172181481150E-17, 1.000000000000000000, -1.765856845898762549E-18 ) ) ;
#7114 = CARTESIAN_POINT ( 'NONE',  ( -12.99553232110414314, 48.77386654458962312, -1.763749038303048460E-15 ) ) ;
#7115 = EDGE_CURVE ( 'NONE', #11396, #11894, #2699, .T. ) ;
#7116 = EDGE_CURVE ( 'NONE', #2454, #283, #11955, .T. ) ;
#7117 = EDGE_LOOP ( 'NONE', ( #6374, #1709, #1571, #12818 ) ) ;
#7118 = DIRECTION ( 'NONE',  ( 1.000000000000000000, 0.000000000000000000, 0.000000000000000000 ) ) ;
#7119 = VECTOR ( 'NONE', #1883, 1000.000000000000000 ) ;
#7120 = VERTEX_POINT ( 'NONE', #11949 ) ;
#7121 = CYLINDRICAL_SURFACE ( 'NONE', #2469, 25.50000000002549783 ) ;
#7122 = EDGE_CURVE ( 'NONE', #11079, #5471, #4082, .T. ) ;
#7123 = EDGE_CURVE ( 'NONE', #6716, #3641, #8345, .T. ) ;
#7124 = ORIENTED_EDGE ( 'NONE', *, *, #704, .F. ) ;
#7125 = ORIENTED_EDGE ( 'NONE', *, *, #1794, .F. ) ;
#7126 = DIRECTION ( 'NONE',  ( -2.797435172181481150E-17, 1.000000000000000000, -1.765856845898762549E-18 ) ) ;
#7127 = DIRECTION ( 'NONE',  ( 1.000000000000000000, 0.000000000000000000, 0.000000000000000000 ) ) ;
#7128 = CARTESIAN_POINT ( 'NONE',  ( 12.93801431150394521, -134.6363636363615797, -1.977757875720894898 ) ) ;
#7129 = CARTESIAN_POINT ( 'NONE',  ( 25.00000000000000355, 120.0000000000000284, 0.5000000000000000000 ) ) ;
#7130 = CARTESIAN_POINT ( 'NONE',  ( -10.69381717166375800, -21.56444287793185310, 21.38763434332750890 ) ) ;
#7131 = CARTESIAN_POINT ( 'NONE',  ( 15.29705854078140348, -29.33764382806072746, 1.923489752901241150E-15 ) ) ;
#7132 = EDGE_CURVE ( 'NONE', #11767, #13355, #3256, .T. ) ;
#7133 = UNCERTAINTY_MEASURE_WITH_UNIT (LENGTH_MEASURE( 1.000000000000000082E-05 ), #2760, 'distance_accuracy_value', 'NONE');
#7134 = CARTESIAN_POINT ( 'NONE',  ( -11.81226048336477064, -40.00941361824966691, 23.62452096672953061 ) ) ;
#7135 = EDGE_CURVE ( 'NONE', #3214, #8349, #1169, .T. ) ;
#7136 = CIRCLE ( 'NONE', #10487, 2.000000000000000000 ) ;
#7137 = ORIENTED_EDGE ( 'NONE', *, *, #13115, .T. ) ;
#7138 = EDGE_CURVE ( 'NONE', #470, #1947, #9497, .T. ) ;
#7139 = AXIS2_PLACEMENT_3D ( 'NONE', #526, #3653, #8084 ) ;
#7140 = EDGE_CURVE ( 'NONE', #768, #1226, #5581, .T. ) ;
#7141 = ORIENTED_EDGE ( 'NONE', *, *, #9869, .T. ) ;
#7142 = CARTESIAN_POINT ( 'NONE',  ( 10.69381717166375800, -12.13966492792242846, 1.341722361464477482E-15 ) ) ;
#7143 = CIRCLE ( 'NONE', #4220, 8.385254915620294014 ) ;
#7144 = CARTESIAN_POINT ( 'NONE',  ( 34.33153323985096250, 107.9636705364999472, 1.438784920770795894 ) ) ;
#7145 = CARTESIAN_POINT ( 'NONE',  ( -0.1852015970780942489, -159.9999997928953235, 1.488522644435750886 ) ) ;
#7146 = DIRECTION ( 'NONE',  ( -1.000000000000000000, 0.000000000000000000, 0.000000000000000000 ) ) ;
#7147 = CARTESIAN_POINT ( 'NONE',  ( 6.692989812469433808, -97.14474235384638234, 4.437126219143910255 ) ) ;
#7148 = EDGE_CURVE ( 'NONE', #6779, #6795, #2449, .T. ) ;
#7149 = DIRECTION ( 'NONE',  ( 0.9928035427100112553, 0.1197544386753605361, 9.637352644305958814E-17 ) ) ;
#7150 = ORIENTED_EDGE ( 'NONE', *, *, #796, .F. ) ;
#7151 = EDGE_CURVE ( 'NONE', #4459, #4900, #6494, .T. ) ;
#7152 = EDGE_LOOP ( 'NONE', ( #48, #1664, #2593, #11540 ) ) ;
#7153 = CIRCLE ( 'NONE', #6482, 4.999999999999998224 ) ;
#7154 = FACE_OUTER_BOUND ( 'NONE', #1164, .T. ) ;
#7155 = CARTESIAN_POINT ( 'NONE',  ( 14.13596196814457784, -39.17949320881311337, -28.27192393628913436 ) ) ;
#7156 = ORIENTED_EDGE ( 'NONE', *, *, #12370, .F. ) ;
#7157 = CYLINDRICAL_SURFACE ( 'NONE', #978, 24.99999999999998934 ) ;
#7158 = DIRECTION ( 'NONE',  ( -6.158143864569485777E-17, -2.736152283717910599E-16, 1.000000000000000000 ) ) ;
#7159 = CARTESIAN_POINT ( 'NONE',  ( -14.37641089434894326, -21.93614314624077721, 6.343488216808987445 ) ) ;
#7160 = CARTESIAN_POINT ( 'NONE',  ( -35.00000000000000000, -4.286263797015736496E-15, 7.500000000000000000 ) ) ;
#7161 = AXIS2_PLACEMENT_3D ( 'NONE', #4218, #13673, #2976 ) ;
#7162 = CARTESIAN_POINT ( 'NONE',  ( -1.375500123858559354, -148.4763468619591151, -1.574495689507027896 ) ) ;
#7163 = DIRECTION ( 'NONE',  ( 0.000000000000000000, 0.000000000000000000, 1.000000000000000000 ) ) ;
#7164 = CIRCLE ( 'NONE', #1824, 25.00000000000000711 ) ;
#7165 = CIRCLE ( 'NONE', #1125, 8.385254915620294014 ) ;
#7166 = ORIENTED_EDGE ( 'NONE', *, *, #11337, .F. ) ;
#7167 = VERTEX_POINT ( 'NONE', #3890 ) ;
#7168 = CARTESIAN_POINT ( 'NONE',  ( -1.705970724789718451, -139.6653734298945722, -2.453391655664824089 ) ) ;
#7169 = CARTESIAN_POINT ( 'NONE',  ( -12.99553232110413958, 39.34908859458022334, 25.99106464220826496 ) ) ;
#7170 =( GEOMETRIC_REPRESENTATION_CONTEXT ( 3 ) GLOBAL_UNCERTAINTY_ASSIGNED_CONTEXT ( ( #6861 ) ) GLOBAL_UNIT_ASSIGNED_CONTEXT ( ( #155, #12852, #1130 ) ) REPRESENTATION_CONTEXT ( 'NONE', 'WORKASPACE' ) );
#7171 = CARTESIAN_POINT ( 'NONE',  ( 0.8657135605078067897, -80.00115760430779233, 9.969076801623804940 ) ) ;
#7172 = DIRECTION ( 'NONE',  ( -0.000000000000000000, -0.000000000000000000, -1.000000000000000000 ) ) ;
#7173 = DIRECTION ( 'NONE',  ( -2.797435172181481150E-17, 1.000000000000000000, -1.765856845898762549E-18 ) ) ;
#7174 = VECTOR ( 'NONE', #10491, 1000.000000000000114 ) ;
#7175 = TOROIDAL_SURFACE ( 'NONE', #10978, 22.49999999999998934, 5.000000000000000000 ) ;
#7176 = LINE ( 'NONE', #10343, #6037 ) ;
#7177 = CARTESIAN_POINT ( 'NONE',  ( -15.29705854078139637, 74.33491362204294717, -1.312648161087776599E-16 ) ) ;
#7178 = CARTESIAN_POINT ( 'NONE',  ( 0.9875500501441598633, -80.00464164738322381, -10.06307372056550342 ) ) ;
#7179 = FACE_OUTER_BOUND ( 'NONE', #10615, .T. ) ;
#7180 = CARTESIAN_POINT ( 'NONE',  ( 0.000000000000000000, 71.01020514433645303, 0.5000000000000000000 ) ) ;
#7181 = CARTESIAN_POINT ( 'NONE',  ( -18.99432778721694604, 26.96223687785629508, -6.295342420724992394 ) ) ;
#7182 = CARTESIAN_POINT ( 'NONE',  ( 8.385254915620292238, 31.55439052270045508, 16.77050983124059513 ) ) ;
#7183 = AXIS2_PLACEMENT_3D ( 'NONE', #12730, #6272, #5212 ) ;
#7184 =( BOUNDED_SURFACE ( )  B_SPLINE_SURFACE ( 3, 3, ( 
 ( #11358, #8906, #10103, #4694 ),
 ( #2602, #9052, #2742, #9959 ),
 ( #514, #12355, #2808, #5680 ),
 ( #11078, #11153, #8002, #366 ) ),
 .UNSPECIFIED., .F., .F., .T. ) 
 B_SPLINE_SURFACE_WITH_KNOTS ( ( 4, 4 ),
 ( 4, 4 ),
 ( 0.000000000000000000, 1.000000000000000000 ),
 ( 0.000000000000000000, 1.000000000000000000 ),
 .UNSPECIFIED. ) 
 GEOMETRIC_REPRESENTATION_ITEM ( )  RATIONAL_B_SPLINE_SURFACE ( (
 ( 1.000000000000000000, 0.3333333333333334259, 0.3333333333333334259, 1.000000000000000000),
 ( 1.000000000000000000, 0.3333333333333334259, 0.3333333333333334259, 1.000000000000000000),
 ( 1.000000000000000000, 0.3333333333333334259, 0.3333333333333334259, 1.000000000000000000),
 ( 1.000000000000000000, 0.3333333333333334259, 0.3333333333333334259, 1.000000000000000000) ) ) 
 REPRESENTATION_ITEM ( '' )  SURFACE ( )  );
#7185 = CARTESIAN_POINT ( 'NONE',  ( -10.00000000000000711, 139.9999999999999716, 0.5000000000000000000 ) ) ;
#7186 = CIRCLE ( 'NONE', #1598, 12.49999999999999289 ) ;
#7187 = ORIENTED_EDGE ( 'NONE', *, *, #4727, .T. ) ;
#7188 = AXIS2_PLACEMENT_3D ( 'NONE', #7838, #9389, #12479 ) ;
#7189 = DIRECTION ( 'NONE',  ( -1.000000000000000000, 0.000000000000000000, 0.000000000000000000 ) ) ;
#7190 = DIRECTION ( 'NONE',  ( 0.9928035427100112553, 0.1197544386753605361, 9.637352644305958814E-17 ) ) ;
#7191 = CYLINDRICAL_SURFACE ( 'NONE', #8844, 15.29705854078139105 ) ;
#7192 = VERTEX_POINT ( 'NONE', #10346 ) ;
#7193 = CARTESIAN_POINT ( 'NONE',  ( -4.363680981163685857, 91.46147893603955481, -2.443653808501017544 ) ) ;
#7194 = CARTESIAN_POINT ( 'NONE',  ( -15.34996685542352424, -16.25414556851945491, -3.363331797608928309 ) ) ;
#7195 = ADVANCED_FACE ( 'NONE', ( #4812 ), #11190, .F. ) ;
#7196 = EDGE_CURVE ( 'NONE', #12718, #6056, #2915, .T. ) ;
#7197 = CARTESIAN_POINT ( 'NONE',  ( 4.154595973944828380, -61.00000000000013500, -0.9946518452611575745 ) ) ;
#7198 = VECTOR ( 'NONE', #5277, 1000.000000000000000 ) ;
#7199 = VECTOR ( 'NONE', #7792, 1000.000000000000000 ) ;
#7200 = CARTESIAN_POINT ( 'NONE',  ( -15.29705854078139282, 47.94714734142005597, -2.042684974582087312E-15 ) ) ;
#7201 = CARTESIAN_POINT ( 'NONE',  ( 13.79311422413708499, -100.0000000000000000, 7.500000000000000000 ) ) ;
#7202 = CARTESIAN_POINT ( 'NONE',  ( 10.69346802281034670, 77.87317997377837742, 0.000000000000000000 ) ) ;
#7203 = AXIS2_PLACEMENT_3D ( 'NONE', #13616, #3965, #13679 ) ;
#7204 = CARTESIAN_POINT ( 'NONE',  ( -3.918572219198208639, -82.19108314072666133, 8.951287372965479605 ) ) ;
#7205 = EDGE_CURVE ( 'NONE', #5202, #1244, #10507, .T. ) ;
#7206 = VERTEX_POINT ( 'NONE', #9089 ) ;
#7207 = CARTESIAN_POINT ( 'NONE',  ( -8.385254915620286909, -22.36966495935058319, -16.77050983124058092 ) ) ;
#7208 = ADVANCED_FACE ( 'NONE', ( #4944 ), #10063, .F. ) ;
#7209 = CARTESIAN_POINT ( 'NONE',  ( 55.16425081158429577, -10.83695794929874090, 2.499999999999998224 ) ) ;
#7210 = CARTESIAN_POINT ( 'NONE',  ( 34.25812584745457201, 108.1980041606221050, 0.5000000000000000000 ) ) ;
#7211 = EDGE_CURVE ( 'NONE', #11499, #9709, #7111, .T. ) ;
#7212 = DIRECTION ( 'NONE',  ( -6.158143864569485777E-17, -2.736152283717910599E-16, 1.000000000000000000 ) ) ;
#7213 = ADVANCED_FACE ( 'NONE', ( #4874 ), #8035, .F. ) ;
#7214 = CARTESIAN_POINT ( 'NONE',  ( 2.824482778608038647, -140.8717184737295440, 0.1012005756595079214 ) ) ;
#7215 = CARTESIAN_POINT ( 'NONE',  ( 10.00000000000000711, 139.9999999999999716, 2.500000000000000000 ) ) ;
#7216 = EDGE_LOOP ( 'NONE', ( #9305, #4570, #10195, #7745 ) ) ;
#7217 = ORIENTED_EDGE ( 'NONE', *, *, #801, .T. ) ;
#7218 = ORIENTED_EDGE ( 'NONE', *, *, #11733, .F. ) ;
#7219 = CARTESIAN_POINT ( 'NONE',  ( -35.00000000000000000, -4.286263797015736496E-15, 4.000000000000000000 ) ) ;
#7220 = ORIENTED_EDGE ( 'NONE', *, *, #13589, .T. ) ;
#7221 = DIRECTION ( 'NONE',  ( -0.000000000000000000, -0.000000000000000000, -1.000000000000000000 ) ) ;
#7222 = EDGE_CURVE ( 'NONE', #13399, #1557, #11417, .T. ) ;
#7223 = ORIENTED_EDGE ( 'NONE', *, *, #10268, .T. ) ;
#7224 = FACE_OUTER_BOUND ( 'NONE', #11689, .T. ) ;
#7225 = ORIENTED_EDGE ( 'NONE', *, *, #12861, .F. ) ;
#7226 = DIRECTION ( 'NONE',  ( -2.797435172181481150E-17, 1.000000000000000000, -1.765856845898762549E-18 ) ) ;
#7227 = DIRECTION ( 'NONE',  ( -1.000000000000000000, 0.000000000000000000, 0.000000000000000000 ) ) ;
#7228 = CARTESIAN_POINT ( 'NONE',  ( 34.99999999999958789, 1.063887963769481123E-13, 12.50000000000000000 ) ) ;
#7229 = FACE_OUTER_BOUND ( 'NONE', #1731, .T. ) ;
#7230 = ADVANCED_FACE ( 'NONE', ( #5786 ), #2776, .T. ) ;
#7231 = CARTESIAN_POINT ( 'NONE',  ( 15.29705854078139105, 27.21102387199583816, 1.823632900916640874E-15 ) ) ;
#7232 = VECTOR ( 'NONE', #8123, 1000.000000000000000 ) ;
#7233 = CARTESIAN_POINT ( 'NONE',  ( 5.702026264667728661, -116.1006108127829606, 0.07857520267129523839 ) ) ;
#7234 = DIRECTION ( 'NONE',  ( -0.8000000000000008216, -0.5999999999999988676, 0.000000000000000000 ) ) ;
#7235 = VERTEX_POINT ( 'NONE', #12315 ) ;
#7236 = EDGE_LOOP ( 'NONE', ( #4862, #12346, #2013, #12919 ) ) ;
#7237 = ORIENTED_EDGE ( 'NONE', *, *, #1948, .F. ) ;
#7238 = ORIENTED_EDGE ( 'NONE', *, *, #7464, .F. ) ;
#7239 = AXIS2_PLACEMENT_3D ( 'NONE', #4637, #771, #2944 ) ;
#7240 = FACE_OUTER_BOUND ( 'NONE', #11558, .T. ) ;
#7241 = DIRECTION ( 'NONE',  ( 1.000000000000000000, 4.625929269271489266E-15, 0.000000000000000000 ) ) ;
#7242 = CARTESIAN_POINT ( 'NONE',  ( 6.017021975735540984, -95.62437285806116449, 5.547819245424533641 ) ) ;
#7243 = CARTESIAN_POINT ( 'NONE',  ( -0.03865624730777729445, -158.0606060610036820, -1.868422726202614959 ) ) ;
#7244 = CARTESIAN_POINT ( 'NONE',  ( 22.00000000000000711, -100.0000000000000000, 2.694222958124176809E-15 ) ) ;
#7245 = DIRECTION ( 'NONE',  ( -1.000000000000000000, 0.000000000000000000, 0.000000000000000000 ) ) ;
#7246 = CARTESIAN_POINT ( 'NONE',  ( 38.81043356982896597, -18.35771219435081392, -2.500000000000004441 ) ) ;
#7247 = CIRCLE ( 'NONE', #4797, 8.385254915620292238 ) ;
#7248 = CARTESIAN_POINT ( 'NONE',  ( 25.00000000000001776, -99.15310334213020838, 3.061571689641656246E-15 ) ) ;
#7249 = CARTESIAN_POINT ( 'NONE',  ( -2.517691654963332357E-15, 90.00000000000000000, -1.589271161308885878E-16 ) ) ;
#7250 = AXIS2_PLACEMENT_3D ( 'NONE', #7788, #12296, #6749 ) ;
#7251 = DIRECTION ( 'NONE',  ( 0.8907235428302444635, 0.4545454545454587492, 0.000000000000000000 ) ) ;
#7252 = ORIENTED_EDGE ( 'NONE', *, *, #8750, .F. ) ;
#7253 = CARTESIAN_POINT ( 'NONE',  ( 25.00000000000000355, 120.0000000000000284, -2.500000000000000000 ) ) ;
#7254 = CARTESIAN_POINT ( 'NONE',  ( -3.606245374342868626, -157.8181818183407756, 2.267989313195203138 ) ) ;
#7255 = ORIENTED_EDGE ( 'NONE', *, *, #9852, .T. ) ;
#7256 = CARTESIAN_POINT ( 'NONE',  ( -10.69381717166375800, -12.13966492792242846, 21.38763434332751245 ) ) ;
#7257 = ORIENTED_EDGE ( 'NONE', *, *, #13518, .T. ) ;
#7258 = AXIS2_PLACEMENT_3D ( 'NONE', #13110, #5577, #341 ) ;
#7259 = CARTESIAN_POINT ( 'NONE',  ( -4.330127018922195425, 92.00000000000000000, -2.500000000000000000 ) ) ;
#7260 = CARTESIAN_POINT ( 'NONE',  ( -15.29705854078140170, -29.33764382806072746, 5.180607919632063331E-17 ) ) ;
#7261 = PLANE ( 'NONE',  #227 ) ;
#7262 = CARTESIAN_POINT ( 'NONE',  ( -6.062451257354288359, -129.7272727272762154, 11.56901651898807160 ) ) ;
#7263 = B_SPLINE_CURVE_WITH_KNOTS ( 'NONE', 3,
 ( #10888, #259, #1171, #8793 ),
 .UNSPECIFIED., .F., .F.,
 ( 4, 4 ),
 ( 0.000000000000000000, 1.000000000000000000 ),
 .UNSPECIFIED. ) ;
#7264 = CARTESIAN_POINT ( 'NONE',  ( 8.385254915620292238, 59.82872437272870769, 9.189312520034297072E-16 ) ) ;
#7265 = DIRECTION ( 'NONE',  ( -6.158143864569485777E-17, -2.736152283717910599E-16, 1.000000000000000000 ) ) ;
#7266 = DIRECTION ( 'NONE',  ( -0.000000000000000000, -0.000000000000000000, -1.000000000000000000 ) ) ;
#7267 = CIRCLE ( 'NONE', #13325, 18.74900000001875355 ) ;
#7268 = CARTESIAN_POINT ( 'NONE',  ( 1.922734475756564121E-15, -100.0000000000000000, -15.70031846811053455 ) ) ;
#7269 = CIRCLE ( 'NONE', #5033, 15.29705854078139105 ) ;
#7270 = EDGE_CURVE ( 'NONE', #10317, #4734, #4453, .T. ) ;
#7271 = VERTEX_POINT ( 'NONE', #2839 ) ;
#7272 = AXIS2_PLACEMENT_3D ( 'NONE', #13601, #3954, #5076 ) ;
#7273 = ORIENTED_EDGE ( 'NONE', *, *, #4649, .F. ) ;
#7274 = CARTESIAN_POINT ( 'NONE',  ( 15.29705854078140348, -19.91286587805129926, -30.59411708156278920 ) ) ;
#7275 = CIRCLE ( 'NONE', #9964, 40.00000000000001421 ) ;
#7276 = DIRECTION ( 'NONE',  ( -0.000000000000000000, -0.000000000000000000, -1.000000000000000000 ) ) ;
#7277 = CARTESIAN_POINT ( 'NONE',  ( 34.27523635402735636, 108.1397967565350200, 0.9870360185550118848 ) ) ;
#7278 = CARTESIAN_POINT ( 'NONE',  ( 12.99579180576517068, -1.889935973073298081, -25.99158361153033070 ) ) ;
#7279 = FACE_OUTER_BOUND ( 'NONE', #13188, .T. ) ;
#7280 = DIRECTION ( 'NONE',  ( -0.000000000000000000, -0.000000000000000000, -1.000000000000000000 ) ) ;
#7281 = EDGE_CURVE ( 'NONE', #7540, #3278, #8056, .T. ) ;
#7282 = ADVANCED_FACE ( 'NONE', ( #613 ), #13541, .F. ) ;
#7283 = EDGE_LOOP ( 'NONE', ( #1105, #11294, #13573, #912 ) ) ;
#7284 = AXIS2_PLACEMENT_3D ( 'NONE', #10046, #9979, #9000 ) ;
#7285 = EDGE_CURVE ( 'NONE', #5648, #9044, #7603, .T. ) ;
#7286 = CARTESIAN_POINT ( 'NONE',  ( -2.517691654963332357E-15, 90.00000000000000000, -1.589271161308885878E-16 ) ) ;
#7287 =( GEOMETRIC_REPRESENTATION_CONTEXT ( 3 ) GLOBAL_UNCERTAINTY_ASSIGNED_CONTEXT ( ( #1252 ) ) GLOBAL_UNIT_ASSIGNED_CONTEXT ( ( #1376, #12034, #6778 ) ) REPRESENTATION_CONTEXT ( 'NONE', 'WORKASPACE' ) );
#7288 = EDGE_CURVE ( 'NONE', #7028, #6075, #7826, .T. ) ;
#7289 = CIRCLE ( 'NONE', #4371, 2.000000000000003109 ) ;
#7290 = EDGE_CURVE ( 'NONE', #11147, #13800, #5139, .T. ) ;
#7291 = EDGE_LOOP ( 'NONE', ( #1000, #9072, #7451, #11184, #10709, #10787, #9235 ) ) ;
#7292 = DIRECTION ( 'NONE',  ( -1.000000000000000000, 0.000000000000000000, 0.000000000000000000 ) ) ;
#7293 = CARTESIAN_POINT ( 'NONE',  ( 1.416598489609834699, -78.09090909090815558, 10.12631592825928273 ) ) ;
#7294 = ORIENTED_EDGE ( 'NONE', *, *, #10894, .T. ) ;
#7295 = DIRECTION ( 'NONE',  ( -1.000000000000000000, 0.000000000000000000, -0.000000000000000000 ) ) ;
#7296 = CARTESIAN_POINT ( 'NONE',  ( 4.974937185533097050, 90.00000000000000000, 0.5000000000000000000 ) ) ;
#7297 = AXIS2_PLACEMENT_3D ( 'NONE', #9270, #10460, #13587 ) ;
#7298 = FACE_OUTER_BOUND ( 'NONE', #10434, .T. ) ;
#7299 = FACE_OUTER_BOUND ( 'NONE', #8622, .T. ) ;
#7300 = CARTESIAN_POINT ( 'NONE',  ( -15.29705854078139460, -18.02629830864596627, 3.183186227453577089E-17 ) ) ;
#7301 = CARTESIAN_POINT ( 'NONE',  ( 5.749669232646114736, -115.6779247526754091, -0.2475080363690762286 ) ) ;
#7302 = DIRECTION ( 'NONE',  ( 0.8000000000000008216, 0.5999999999999988676, -4.163336342344329138E-15 ) ) ;
#7303 = ORIENTED_EDGE ( 'NONE', *, *, #13423, .F. ) ;
#7304 = ORIENTED_EDGE ( 'NONE', *, *, #5573, .F. ) ;
#7305 = ORIENTED_EDGE ( 'NONE', *, *, #867, .F. ) ;
#7306 = ADVANCED_FACE ( 'NONE', ( #12389 ), #11487, .T. ) ;
#7307 = ORIENTED_EDGE ( 'NONE', *, *, #1730, .T. ) ;
#7308 = ADVANCED_FACE ( 'NONE', ( #5209 ), #12665, .F. ) ;
#7309 = FACE_OUTER_BOUND ( 'NONE', #11802, .T. ) ;
#7310 = CARTESIAN_POINT ( 'NONE',  ( 2.082709946752197006, -80.78332142495241897, -9.792949010885818595 ) ) ;
#7311 = FACE_OUTER_BOUND ( 'NONE', #8319, .T. ) ;
#7312 = CARTESIAN_POINT ( 'NONE',  ( -15.29705854078139282, 46.06057977201469100, -8.133639011647813827E-17 ) ) ;
#7313 = CARTESIAN_POINT ( 'NONE',  ( 35.45454545454547457, 140.4866414850956744, 0.5000000000000000000 ) ) ;
#7314 = CARTESIAN_POINT ( 'NONE',  ( -36.36363636363635976, 142.2680885707561629, 2.500000000000000000 ) ) ;
#7315 = VECTOR ( 'NONE', #1381, 1000.000000000000000 ) ;
#7316 = CARTESIAN_POINT ( 'NONE',  ( -22.42156014662057473, -97.00000000000000000, 7.500000000000000000 ) ) ;
#7317 = FACE_OUTER_BOUND ( 'NONE', #3583, .T. ) ;
#7318 = CARTESIAN_POINT ( 'NONE',  ( 52.49999999999999289, 120.0000000000000142, 2.499999999999999556 ) ) ;
#7319 = ORIENTED_EDGE ( 'NONE', *, *, #10303, .T. ) ;
#7320 = CARTESIAN_POINT ( 'NONE',  ( 1.133743435585240489, -129.7272727272670352, -4.472427317383721679 ) ) ;
#7321 = EDGE_CURVE ( 'NONE', #8040, #13223, #8287, .T. ) ;
#7322 = ORIENTED_EDGE ( 'NONE', *, *, #4539, .T. ) ;
#7323 = CARTESIAN_POINT ( 'NONE',  ( 8.385254915620294014, -12.94488700934118341, 2.053795118489800793E-15 ) ) ;
#7324 = ORIENTED_EDGE ( 'NONE', *, *, #7477, .T. ) ;
#7325 = DIRECTION ( 'NONE',  ( 6.158143864569485777E-17, 2.736152283717910599E-16, -1.000000000000000000 ) ) ;
#7326 = CARTESIAN_POINT ( 'NONE',  ( 32.61455173758670867, 25.38817907193537593, 2.500000000000007105 ) ) ;
#7327 = CARTESIAN_POINT ( 'NONE',  ( 8.355259928129500580, -76.12121212035069107, 3.018973157362855986 ) ) ;
#7328 = CARTESIAN_POINT ( 'NONE',  ( 11.42080557901028293, -157.8181818180634366, -3.873507862844141947 ) ) ;
#7329 = CYLINDRICAL_SURFACE ( 'NONE', #13717, 66.25000000000044054 ) ;
#7330 = FACE_OUTER_BOUND ( 'NONE', #1025, .T. ) ;
#7331 = DIRECTION ( 'NONE',  ( 2.797435172181480534E-17, -1.000000000000000000, 1.765856845898762164E-18 ) ) ;
#7332 = CARTESIAN_POINT ( 'NONE',  ( 22.42156014662059249, -97.00000000000000000, -7.500000000000000000 ) ) ;
#7333 = ORIENTED_EDGE ( 'NONE', *, *, #11295, .F. ) ;
#7334 = ORIENTED_EDGE ( 'NONE', *, *, #1742, .T. ) ;
#7335 = DIRECTION ( 'NONE',  ( 0.9960067511297463483, -0.08927794634716620936, 4.626175998653454121E-17 ) ) ;
#7336 = EDGE_CURVE ( 'NONE', #2480, #12324, #12992, .T. ) ;
#7337 = CARTESIAN_POINT ( 'NONE',  ( 34.79486456029760433, 106.9754367860671778, 2.376147960742919452 ) ) ;
#7338 = CARTESIAN_POINT ( 'NONE',  ( -2.200973885217364349E-15, 78.67828027274755698, -1.389345798431728350E-16 ) ) ;
#7339 = CARTESIAN_POINT ( 'NONE',  ( 23.18128365339294916, -22.59575057217061200, -2.500000000000006217 ) ) ;
#7340 = VECTOR ( 'NONE', #844, 1000.000000000000000 ) ;
#7341 = DIRECTION ( 'NONE',  ( -0.5999999999999989786, -0.8000000000000008216, 0.000000000000000000 ) ) ;
#7342 = AXIS2_PLACEMENT_3D ( 'NONE', #10992, #7559, #6520 ) ;
#7343 = EDGE_LOOP ( 'NONE', ( #1843, #8897, #12421, #12011 ) ) ;
#7344 = ORIENTED_EDGE ( 'NONE', *, *, #12547, .T. ) ;
#7345 = CARTESIAN_POINT ( 'NONE',  ( 38.24615002434714484, 18.46584715143433542, -2.499999999999993783 ) ) ;
#7346 = VECTOR ( 'NONE', #349, 1000.000000000000000 ) ;
#7347 = ORIENTED_EDGE ( 'NONE', *, *, #11809, .T. ) ;
#7348 = DIRECTION ( 'NONE',  ( 1.000000000000000000, 2.081668171172168119E-15, 0.000000000000000000 ) ) ;
#7349 = ORIENTED_EDGE ( 'NONE', *, *, #8743, .F. ) ;
#7350 = CYLINDRICAL_SURFACE ( 'NONE', #4105, 9.000000000008999024 ) ;
#7351 = EDGE_CURVE ( 'NONE', #11251, #3661, #945, .T. ) ;
#7352 = CARTESIAN_POINT ( 'NONE',  ( -7.616846500253796393, -85.78354978338798276, 7.024694013272235971 ) ) ;
#7353 = CARTESIAN_POINT ( 'NONE',  ( -36.50000000000000000, 113.0000000000000142, 2.499999999999999556 ) ) ;
#7354 = ADVANCED_FACE ( 'NONE', ( #12728 ), #7590, .T. ) ;
#7355 = DIRECTION ( 'NONE',  ( -0.2228746399763463781, 0.9748471135800803600, 2.544396799259399212E-16 ) ) ;
#7356 = CARTESIAN_POINT ( 'NONE',  ( 10.69346802281034314, 21.32451227372186864, 0.000000000000000000 ) ) ;
#7357 = CARTESIAN_POINT ( 'NONE',  ( -24.99999999999999645, -99.74063674767198506, 4.228074540580154306 ) ) ;
#7358 = CARTESIAN_POINT ( 'NONE',  ( 1.187907395172932673E-14, -97.00000000000000000, 0.000000000000000000 ) ) ;
#7359 = CARTESIAN_POINT ( 'NONE',  ( -1.327769271380126570, -103.0493006173539641, -7.164857848410852270 ) ) ;
#7360 = EDGE_CURVE ( 'NONE', #9139, #2097, #3044, .T. ) ;
#7361 = FACE_OUTER_BOUND ( 'NONE', #2693, .T. ) ;
#7362 = ORIENTED_EDGE ( 'NONE', *, *, #13614, .F. ) ;
#7363 = AXIS2_PLACEMENT_3D ( 'NONE', #4213, #1981, #12657 ) ;
#7364 = ORIENTED_EDGE ( 'NONE', *, *, #1364, .F. ) ;
#7365 = ORIENTED_EDGE ( 'NONE', *, *, #9772, .F. ) ;
#7366 = AXIS2_PLACEMENT_3D ( 'NONE', #4039, #2073, #6083 ) ;
#7367 = CARTESIAN_POINT ( 'NONE',  ( 21.34086416022640265, 21.53318388236929692, 2.500000000000005329 ) ) ;
#7368 = DIRECTION ( 'NONE',  ( -0.4545454545454548634, 0.8907235428302464619, 0.000000000000000000 ) ) ;
#7369 = EDGE_LOOP ( 'NONE', ( #1491, #11567, #11249, #10871 ) ) ;
#7370 = DIRECTION ( 'NONE',  ( -0.000000000000000000, -0.000000000000000000, -1.000000000000000000 ) ) ;
#7371 = CARTESIAN_POINT ( 'NONE',  ( -5.489740287354453407, -114.7850684598158892, -2.013460231478539253 ) ) ;
#7372 = EDGE_CURVE ( 'NONE', #9123, #13392, #12555, .T. ) ;
#7373 = VECTOR ( 'NONE', #1718, 1000.000000000000000 ) ;
#7374 = CARTESIAN_POINT ( 'NONE',  ( 11.81226048336477064, -40.00941361824963849, 0.000000000000000000 ) ) ;
#7375 = EDGE_CURVE ( 'NONE', #2284, #10314, #10083, .T. ) ;
#7376 = CARTESIAN_POINT ( 'NONE',  ( 15.29705854078139282, 19.67281349139177138, -30.59411708156276788 ) ) ;
#7377 = CARTESIAN_POINT ( 'NONE',  ( 8.385254915620294014, 3.280056672672171381, 1.027013741517443780E-15 ) ) ;
#7378 = AXIS2_PLACEMENT_3D ( 'NONE', #7659, #6611, #13164 ) ;
#7379 = CARTESIAN_POINT ( 'NONE',  ( 34.99999999999958789, 1.104930248025249758E-13, -2.499999999999999112 ) ) ;
#7380 = EDGE_CURVE ( 'NONE', #4069, #13581, #9561, .T. ) ;
#7381 = CARTESIAN_POINT ( 'NONE',  ( -15.29705854078139105, 29.09759144140119957, -1.976113739925688312E-15 ) ) ;
#7382 = EDGE_CURVE ( 'NONE', #2641, #780, #8711, .T. ) ;
#7383 = EDGE_LOOP ( 'NONE', ( #982, #11186, #7102, #9756 ) ) ;
#7384 = CARTESIAN_POINT ( 'NONE',  ( -35.45454545454546036, 140.4866414850956744, -0.5000000000000000000 ) ) ;
#7385 = CARTESIAN_POINT ( 'NONE',  ( 30.68181818181819054, 131.1340442853780530, 2.499999999999999556 ) ) ;
#7386 = PRESENTATION_LAYER_ASSIGNMENT (  '', '', ( #12331 ) ) ;
#7387 = CARTESIAN_POINT ( 'NONE',  ( 4.801896836370951327, -140.5584415584236240, 0.8531065430110326142 ) ) ;
#7388 = CIRCLE ( 'NONE', #11873, 2.000000000000001776 ) ;
#7389 = ORIENTED_EDGE ( 'NONE', *, *, #2653, .T. ) ;
#7390 = TOROIDAL_SURFACE ( 'NONE', #5365, 17.49999999999999645, 5.000000000000000000 ) ;
#7391 = DIRECTION ( 'NONE',  ( -0.000000000000000000, -0.000000000000000000, -1.000000000000000000 ) ) ;
#7392 = ORIENTED_EDGE ( 'NONE', *, *, #2528, .F. ) ;
#7393 = DIRECTION ( 'NONE',  ( 0.000000000000000000, 1.000000000000000000, -0.000000000000000000 ) ) ;
#7394 = CYLINDRICAL_SURFACE ( 'NONE', #11965, 25.50000000002549783 ) ;
#7395 = CARTESIAN_POINT ( 'NONE',  ( 15.49340857339600142, -22.63585399314533575, 2.623848604783063365 ) ) ;
#7396 = EDGE_CURVE ( 'NONE', #1501, #8022, #1324, .T. ) ;
#7397 = CARTESIAN_POINT ( 'NONE',  ( 4.242345193634528222, -72.18181818161869501, 0.3889582016326292302 ) ) ;
#7398 = AXIS2_PLACEMENT_3D ( 'NONE', #7379, #11667, #1991 ) ;
#7399 = CARTESIAN_POINT ( 'NONE',  ( -10.00000000000000711, 140.0000000000000000, 2.500000000000000000 ) ) ;
#7400 = CARTESIAN_POINT ( 'NONE',  ( -10.69381717166375267, 25.55944687211528787, -21.38763434332751601 ) ) ;
#7401 = DIRECTION ( 'NONE',  ( -2.797435172181481150E-17, 1.000000000000000000, -1.765856845898762549E-18 ) ) ;
#7402 = EDGE_CURVE ( 'NONE', #10681, #9187, #9841, .T. ) ;
#7403 = LINE ( 'NONE', #6091, #2756 ) ;
#7404 = CARTESIAN_POINT ( 'NONE',  ( 15.29705854078138216, 17.78624592198638155, 30.59411708156277498 ) ) ;
#7405 = ORIENTED_EDGE ( 'NONE', *, *, #5693, .F. ) ;
#7406 = ADVANCED_BREP_SHAPE_REPRESENTATION ( '', ( #12476, #8193 ), #11552 ) ;
#7407 = CIRCLE ( 'NONE', #4959, 18.74900000001875711 ) ;
#7408 = CIRCLE ( 'NONE', #3159, 5.000000000000004441 ) ;
#7409 = AXIS2_PLACEMENT_3D ( 'NONE', #2149, #7886, #10957 ) ;
#7410 = CIRCLE ( 'NONE', #12126, 9.000000000008999024 ) ;
#7411 = DIRECTION ( 'NONE',  ( 0.000000000000000000, 0.000000000000000000, 1.000000000000000000 ) ) ;
#7412 = ORIENTED_EDGE ( 'NONE', *, *, #5750, .F. ) ;
#7413 = CARTESIAN_POINT ( 'NONE',  ( -2.517691654963332357E-15, 90.00000000000000000, -1.589271161308885878E-16 ) ) ;
#7414 = CARTESIAN_POINT ( 'NONE',  ( 10.69346802281034492, 68.44840202376897764, 2.619144277183853160E-15 ) ) ;
#7415 = B_SPLINE_CURVE_WITH_KNOTS ( 'NONE', 3,
 ( #8535, #11034, #64, #3130 ),
 .UNSPECIFIED., .F., .F.,
 ( 4, 4 ),
 ( 0.000000000000000000, 1.000000000000000000 ),
 .UNSPECIFIED. ) ;
#7416 = LINE ( 'NONE', #4057, #10690 ) ;
#7417 = CARTESIAN_POINT ( 'NONE',  ( 23.44929957547844879, 14.76842309468663750, -2.499999999999996447 ) ) ;
#7418 = CARTESIAN_POINT ( 'NONE',  ( 2.385373235779478573, -133.5189184999073007, -2.750077259266392460 ) ) ;
#7419 = DIRECTION ( 'NONE',  ( -0.000000000000000000, -0.000000000000000000, -1.000000000000000000 ) ) ;
#7420 = EDGE_LOOP ( 'NONE', ( #3446, #8975, #1127, #7949 ) ) ;
#7421 = AXIS2_PLACEMENT_3D ( 'NONE', #10734, #12726, #2115 ) ;
#7422 = VERTEX_POINT ( 'NONE', #11596 ) ;
#7423 = CARTESIAN_POINT ( 'NONE',  ( 35.06230589874905235, 106.5835921350012967, -2.486789939184903986 ) ) ;
#7424 = CARTESIAN_POINT ( 'NONE',  ( -25.00000000000000355, 120.0000000000000142, 2.499999999999999556 ) ) ;
#7425 = VERTEX_POINT ( 'NONE', #873 ) ;
#7426 = DIRECTION ( 'NONE',  ( 0.01532218268402011502, -0.9998826084685129567, -2.891205793291787644E-16 ) ) ;
#7427 = AXIS2_PLACEMENT_3D ( 'NONE', #7228, #789, #5192 ) ;
#7428 = DIRECTION ( 'NONE',  ( 1.000000000000000000, 0.000000000000000000, 0.000000000000000000 ) ) ;
#7429 = CYLINDRICAL_SURFACE ( 'NONE', #12134, 18.74900000001875000 ) ;
#7430 = CARTESIAN_POINT ( 'NONE',  ( 25.00000000000000355, 120.0000000000000284, 0.5000000000000000000 ) ) ;
#7431 = DIRECTION ( 'NONE',  ( 0.4545454545454531425, 0.8907235428302472391, 0.000000000000000000 ) ) ;
#7432 = DIRECTION ( 'NONE',  ( 0.000000000000000000, 1.000000000000000000, 0.000000000000000000 ) ) ;
#7433 = CARTESIAN_POINT ( 'NONE',  ( 0.7638352155348442363, -126.5711838444371296, 4.383014990228201846 ) ) ;
#7434 = DIRECTION ( 'NONE',  ( -2.797435172181481150E-17, 1.000000000000000000, -1.765856845898762549E-18 ) ) ;
#7435 = ORIENTED_EDGE ( 'NONE', *, *, #12611, .T. ) ;
#7436 = ORIENTED_EDGE ( 'NONE', *, *, #11056, .F. ) ;
#7437 = ADVANCED_FACE ( 'NONE', ( #13742 ), #5141, .T. ) ;
#7438 = CARTESIAN_POINT ( 'NONE',  ( 8.385254915620294014, 40.97916847270985130, 2.053795118489800793E-15 ) ) ;
#7439 = EDGE_LOOP ( 'NONE', ( #6852, #7705, #1166, #11822 ) ) ;
#7440 = CYLINDRICAL_SURFACE ( 'NONE', #1024, 18.74900000001875000 ) ;
#7441 = CARTESIAN_POINT ( 'NONE',  ( -1.444477056741696464, -121.1523416466594654, -4.889642476594785236 ) ) ;
#7442 = FACE_OUTER_BOUND ( 'NONE', #9818, .T. ) ;
#7443 = CIRCLE ( 'NONE', #1858, 2.000000000000000000 ) ;
#7444 = CARTESIAN_POINT ( 'NONE',  ( -2.966263562846015667, -142.5800865800325994, -0.5601050917294461140 ) ) ;
#7445 = CARTESIAN_POINT ( 'NONE',  ( 0.000000000000000000, 40.00000000000000000, 20.00000000000000000 ) ) ;
#7446 = CIRCLE ( 'NONE', #2289, 8.385254915620290461 ) ;
#7447 = DIRECTION ( 'NONE',  ( -6.158143864569485777E-17, -2.736152283717910599E-16, 1.000000000000000000 ) ) ;
#7448 = CARTESIAN_POINT ( 'NONE',  ( -2.142312913383871198, -80.12121212121239466, -9.955895698471787014 ) ) ;
#7449 = CARTESIAN_POINT ( 'NONE',  ( 1.119237408740483274E-15, -40.00941361824966691, 7.065089693818133469E-17 ) ) ;
#7450 = CARTESIAN_POINT ( 'NONE',  ( 34.99999999999958789, 1.091249486606660213E-13, 2.500000000000000000 ) ) ;
#7451 = ORIENTED_EDGE ( 'NONE', *, *, #8245, .T. ) ;
#7452 = ADVANCED_FACE ( 'NONE', ( #7179 ), #1851, .T. ) ;
#7453 = VECTOR ( 'NONE', #2445, 1000.000000000000000 ) ;
#7454 = EDGE_LOOP ( 'NONE', ( #4160, #2306, #5571, #8365 ) ) ;
#7455 = EDGE_CURVE ( 'NONE', #5860, #11418, #13482, .T. ) ;
#7456 = CARTESIAN_POINT ( 'NONE',  ( -57.42269783611796186, -167.3636363826522881, 5.376878112289413814 ) ) ;
#7457 = AXIS2_PLACEMENT_3D ( 'NONE', #8838, #3494, #5404 ) ;
#7458 = ADVANCED_FACE ( 'NONE', ( #6746 ), #7717, .T. ) ;
#7459 = ORIENTED_EDGE ( 'NONE', *, *, #5306, .T. ) ;
#7460 = DIRECTION ( 'NONE',  ( -2.797435172181481150E-17, 1.000000000000000000, -1.765856845898762549E-18 ) ) ;
#7461 = EDGE_CURVE ( 'NONE', #7855, #283, #9905, .T. ) ;
#7462 = EDGE_LOOP ( 'NONE', ( #5964, #2401, #12690, #2421 ) ) ;
#7463 = CARTESIAN_POINT ( 'NONE',  ( 26.09988479906369463, 19.17858047941126642, -2.499999999999993783 ) ) ;
#7464 = EDGE_CURVE ( 'NONE', #182, #12385, #7785, .T. ) ;
#7465 = DIRECTION ( 'NONE',  ( -1.000000000000000000, 0.000000000000000000, 0.000000000000000000 ) ) ;
#7466 = CARTESIAN_POINT ( 'NONE',  ( 10.69381717166375623, 25.55944687211528077, 2.619229793989004345E-15 ) ) ;
#7467 = AXIS2_PLACEMENT_3D ( 'NONE', #8214, #855, #5119 ) ;
#7468 = VECTOR ( 'NONE', #11933, 1000.000000000000000 ) ;
#7469 = CARTESIAN_POINT ( 'NONE',  ( 3.373786045844536563, -82.89610389618431441, -3.887588323741812957 ) ) ;
#7470 = FACE_OUTER_BOUND ( 'NONE', #12508, .T. ) ;
#7471 = CARTESIAN_POINT ( 'NONE',  ( -12.99553232110413248, 11.07475474455194053, -25.99106464220827561 ) ) ;
#7472 = DIRECTION ( 'NONE',  ( -0.000000000000000000, -0.000000000000000000, -1.000000000000000000 ) ) ;
#7473 = DIRECTION ( 'NONE',  ( -2.797435172181481150E-17, 1.000000000000000000, -1.765856845898762549E-18 ) ) ;
#7474 = DIRECTION ( 'NONE',  ( 1.000000000000000000, 0.000000000000000000, 0.000000000000000000 ) ) ;
#7475 = VERTEX_POINT ( 'NONE', #4291 ) ;
#7476 = AXIS2_PLACEMENT_3D ( 'NONE', #690, #2718, #9376 ) ;
#7477 = EDGE_CURVE ( 'NONE', #1890, #5237, #6707, .T. ) ;
#7478 = ORIENTED_EDGE ( 'NONE', *, *, #6703, .T. ) ;
#7479 = CYLINDRICAL_SURFACE ( 'NONE', #5875, 8.385254915620295790 ) ;
#7480 = DIRECTION ( 'NONE',  ( 1.000000000000000000, 6.938893903907226405E-16, 0.000000000000000000 ) ) ;
#7481 = CARTESIAN_POINT ( 'NONE',  ( -12.99579180576517068, 54.65873172698324112, -1.784564474948045950E-15 ) ) ;
#7482 = AXIS2_PLACEMENT_3D ( 'NONE', #4433, #8715, #4373 ) ;
#7483 = CARTESIAN_POINT ( 'NONE',  ( -9.636121577330632348, -72.23759218051375797, -2.995460436795389647 ) ) ;
#7484 = CARTESIAN_POINT ( 'NONE',  ( -2.517691654963332357E-15, 90.00000000000000000, -1.589271161308885878E-16 ) ) ;
#7485 = CYLINDRICAL_SURFACE ( 'NONE', #3996, 5.999999999999998224 ) ;
#7486 = AXIS2_PLACEMENT_3D ( 'NONE', #5158, #12887, #12819 ) ;
#7487 = ORIENTED_EDGE ( 'NONE', *, *, #2929, .T. ) ;
#7488 = ORIENTED_EDGE ( 'NONE', *, *, #13161, .F. ) ;
#7489 = ORIENTED_EDGE ( 'NONE', *, *, #7455, .T. ) ;
#7490 = AXIS2_PLACEMENT_3D ( 'NONE', #10483, #12607, #4230 ) ;
#7491 = ADVANCED_FACE ( 'NONE', ( #11930 ), #172, .T. ) ;
#7492 = CARTESIAN_POINT ( 'NONE',  ( 7.679260624019852705E-16, -27.45107625865536605, 4.847467093863555185E-17 ) ) ;
#7493 = AXIS2_PLACEMENT_3D ( 'NONE', #6001, #3672, #2630 ) ;
#7494 = VERTEX_POINT ( 'NONE', #4417 ) ;
#7495 = DIRECTION ( 'NONE',  ( 0.000000000000000000, 0.000000000000000000, 1.000000000000000000 ) ) ;
#7496 = CARTESIAN_POINT ( 'NONE',  ( 0.000000000000000000, 71.01020514433645303, -2.499999999999998668 ) ) ;
#7497 = DIRECTION ( 'NONE',  ( -1.000000000000000000, 0.000000000000000000, 0.000000000000000000 ) ) ;
#7498 = CARTESIAN_POINT ( 'NONE',  ( 34.99999999999958789, 1.091249486606660213E-13, 2.500000000000000000 ) ) ;
#7499 = CARTESIAN_POINT ( 'NONE',  ( -6.370414618488270619, -97.56321138151314187, -4.760973744585681011 ) ) ;
#7500 = DIRECTION ( 'NONE',  ( 0.000000000000000000, 0.000000000000000000, 1.000000000000000000 ) ) ;
#7501 = ORIENTED_EDGE ( 'NONE', *, *, #1543, .F. ) ;
#7502 = ORIENTED_EDGE ( 'NONE', *, *, #5572, .F. ) ;
#7503 = COLOUR_RGB ( '', 0.72549020, 0.75294118, 0.79215686) ;
#7504 = ORIENTED_EDGE ( 'NONE', *, *, #1401, .T. ) ;
#7505 = VECTOR ( 'NONE', #2619, 1000.000000000000000 ) ;
#7506 = CARTESIAN_POINT ( 'NONE',  ( -26.79177319725820894, -26.24642857144861807, -4.000000000000000000 ) ) ;
#7507 = ORIENTED_EDGE ( 'NONE', *, *, #6529, .F. ) ;
#7508 = CARTESIAN_POINT ( 'NONE',  ( 15.29705854078138749, -1.063309978032445091, 30.59411708156277854 ) ) ;
#7509 = AXIS2_PLACEMENT_3D ( 'NONE', #8979, #6725, #5600 ) ;
#7510 = DIRECTION ( 'NONE',  ( 1.000000000000000000, 0.000000000000000000, 0.000000000000000000 ) ) ;
#7511 = CARTESIAN_POINT ( 'NONE',  ( -4.184759487138673961, -117.2897403752749312, -3.654242507195469170 ) ) ;
#7512 = LINE ( 'NONE', #2182, #13700 ) ;
#7513 = CARTESIAN_POINT ( 'NONE',  ( -2.517691654963332357E-15, 90.00000000000000000, -1.589271161308885878E-16 ) ) ;
#7514 = CARTESIAN_POINT ( 'NONE',  ( -2.517691654963332357E-15, 90.00000000000000000, -1.589271161308885878E-16 ) ) ;
#7515 = AXIS2_PLACEMENT_3D ( 'NONE', #11474, #1866, #8118 ) ;
#7516 = CARTESIAN_POINT ( 'NONE',  ( -9.977514653935900313, -69.33333333333061432, -0.8249805266091697620 ) ) ;
#7517 = EDGE_CURVE ( 'NONE', #3806, #9883, #9773, .T. ) ;
#7518 = DIRECTION ( 'NONE',  ( -0.000000000000000000, -0.000000000000000000, 1.000000000000000000 ) ) ;
#7519 = DIRECTION ( 'NONE',  ( -0.5999999999999989786, -0.8000000000000008216, 0.000000000000000000 ) ) ;
#7520 = AXIS2_PLACEMENT_3D ( 'NONE', #7008, #3987, #2077 ) ;
#7521 = FACE_OUTER_BOUND ( 'NONE', #9751, .T. ) ;
#7522 = VERTEX_POINT ( 'NONE', #6666 ) ;
#7523 = ORIENTED_EDGE ( 'NONE', *, *, #2379, .T. ) ;
#7524 = DIRECTION ( 'NONE',  ( 0.9960067511297463483, -0.08927794634716618161, 4.818676322152979407E-17 ) ) ;
#7525 = VERTEX_POINT ( 'NONE', #11796 ) ;
#7526 = DIRECTION ( 'NONE',  ( -0.000000000000000000, -0.000000000000000000, -1.000000000000000000 ) ) ;
#7527 = EDGE_LOOP ( 'NONE', ( #10368, #2417, #12041, #10107 ) ) ;
#7528 = CARTESIAN_POINT ( 'NONE',  ( 1.084353620409068652E-15, -38.76242177807012723, 6.844888786042043893E-17 ) ) ;
#7529 = CARTESIAN_POINT ( 'NONE',  ( 12.99579180576516890, 26.38439787695498495, 3.183050967463142985E-15 ) ) ;
#7530 = CARTESIAN_POINT ( 'NONE',  ( -8.385254915620297567, 90.00000000000000000, -1.589271161308885878E-16 ) ) ;
#7531 = EDGE_CURVE ( 'NONE', #11542, #397, #10313, .T. ) ;
#7532 = CARTESIAN_POINT ( 'NONE',  ( -45.97632359910779343, 102.2167537197081799, 2.499999999999999556 ) ) ;
#7533 = CARTESIAN_POINT ( 'NONE',  ( -15.29705854078138749, 27.21102387199583461, -30.59411708156277854 ) ) ;
#7534 = EDGE_CURVE ( 'NONE', #11046, #10478, #9828, .T. ) ;
#7535 = CARTESIAN_POINT ( 'NONE',  ( 15.29705854078140170, -19.91286587805129926, 1.906846944237140710E-15 ) ) ;
#7536 = PLANE ( 'NONE',  #298 ) ;
#7537 = FACE_OUTER_BOUND ( 'NONE', #9390, .T. ) ;
#7538 = EDGE_CURVE ( 'NONE', #12059, #131, #4936, .T. ) ;
#7539 = ADVANCED_FACE ( 'NONE', ( #12073 ), #519, .F. ) ;
#7540 = VERTEX_POINT ( 'NONE', #7093 ) ;
#7541 = DIRECTION ( 'NONE',  ( 1.000000000000000000, 0.000000000000000000, 0.000000000000000000 ) ) ;
#7542 = ORIENTED_EDGE ( 'NONE', *, *, #255, .T. ) ;
#7543 = CARTESIAN_POINT ( 'NONE',  ( -12.99553232110413958, 67.62342244460847951, -1.830320272959447658E-15 ) ) ;
#7544 = EDGE_CURVE ( 'NONE', #9863, #4263, #994, .T. ) ;
#7545 = DIRECTION ( 'NONE',  ( 1.000000000000000000, 0.000000000000000000, 0.000000000000000000 ) ) ;
#7546 = EDGE_CURVE ( 'NONE', #5181, #8931, #6252, .T. ) ;
#7547 = FACE_OUTER_BOUND ( 'NONE', #13469, .T. ) ;
#7548 = CARTESIAN_POINT ( 'NONE',  ( 8.385254915620290461, 12.70483462268160046, 16.77050983124058803 ) ) ;
#7549 = ADVANCED_FACE ( 'NONE', ( #7229 ), #2925, .T. ) ;
#7550 = ORIENTED_EDGE ( 'NONE', *, *, #6781, .T. ) ;
#7551 = EDGE_CURVE ( 'NONE', #10942, #2744, #11614, .T. ) ;
#7552 = ORIENTED_EDGE ( 'NONE', *, *, #8130, .T. ) ;
#7553 = EDGE_LOOP ( 'NONE', ( #6094, #8853, #7542, #12201 ) ) ;
#7554 = EDGE_LOOP ( 'NONE', ( #3947, #3597, #2329, #6683 ) ) ;
#7555 = CARTESIAN_POINT ( 'NONE',  ( 15.29705854078138927, 76.22148119144830503, -30.59411708156276788 ) ) ;
#7556 = ORIENTED_EDGE ( 'NONE', *, *, #1889, .F. ) ;
#7557 = CARTESIAN_POINT ( 'NONE',  ( 30.72062512117249611, 25.13835616439071785, 0.000000000000000000 ) ) ;
#7558 = CIRCLE ( 'NONE', #3305, 25.00000000000000355 ) ;
#7559 = DIRECTION ( 'NONE',  ( 0.000000000000000000, 0.000000000000000000, 1.000000000000000000 ) ) ;
#7560 = CARTESIAN_POINT ( 'NONE',  ( -6.629834750586161896, -74.11811805074310655, -7.660853594987535153 ) ) ;
#7561 = AXIS2_PLACEMENT_3D ( 'NONE', #9410, #6121, #925 ) ;
#7562 = DIRECTION ( 'NONE',  ( -2.797435172181481150E-17, 1.000000000000000000, -1.765856845898762549E-18 ) ) ;
#7563 = CARTESIAN_POINT ( 'NONE',  ( 3.159504973698678221, 90.09612598291144536, -3.878748273749980768 ) ) ;
#7564 = CARTESIAN_POINT ( 'NONE',  ( -4.875680159242816281, -85.38011053856008914, 8.109980874214908653 ) ) ;
#7565 = LINE ( 'NONE', #3155, #141 ) ;
#7566 = ORIENTED_EDGE ( 'NONE', *, *, #9224, .T. ) ;
#7567 = EDGE_CURVE ( 'NONE', #3229, #12269, #9413, .T. ) ;
#7568 = ORIENTED_EDGE ( 'NONE', *, *, #3281, .F. ) ;
#7569 = ORIENTED_EDGE ( 'NONE', *, *, #8901, .F. ) ;
#7570 = AXIS2_PLACEMENT_3D ( 'NONE', #11344, #5032, #10295 ) ;
#7571 = CIRCLE ( 'NONE', #13678, 25.00000000000000711 ) ;
#7572 = CARTESIAN_POINT ( 'NONE',  ( -8.385254915620294014, 90.00000000000000000, -1.589271161308885878E-16 ) ) ;
#7573 = CARTESIAN_POINT ( 'NONE',  ( 47.16901142695026294, 17.29003067336574517, 2.500000000000005773 ) ) ;
#7574 = VERTEX_POINT ( 'NONE', #8482 ) ;
#7575 = DIRECTION ( 'NONE',  ( -0.2228746399763463781, 0.9748471135800803600, 2.544396799259399212E-16 ) ) ;
#7576 = FILL_AREA_STYLE ('',( #7779 ) ) ;
#7577 = CARTESIAN_POINT ( 'NONE',  ( 1.653273178848927024E-14, -135.0000000000000000, 0.000000000000000000 ) ) ;
#7578 = CARTESIAN_POINT ( 'NONE',  ( -12.99579180576516535, 7.534841976936128560, -3.197093525192043264E-15 ) ) ;
#7579 = CARTESIAN_POINT ( 'NONE',  ( -10.11144051725924520, -69.99977036137985920, 0.2534939247371171822 ) ) ;
#7580 = CARTESIAN_POINT ( 'NONE',  ( -0.1425268984646445858, -158.0606060616233606, 0.6718241418580294111 ) ) ;
#7581 = CARTESIAN_POINT ( 'NONE',  ( -8.804495088766199018, -73.18181818181871279, -4.925729831870038211 ) ) ;
#7582 = CIRCLE ( 'NONE', #13688, 25.50418395392908977 ) ;
#7583 = DIRECTION ( 'NONE',  ( -2.797435172181481150E-17, 1.000000000000000000, -1.765856845898762549E-18 ) ) ;
#7584 = FACE_OUTER_BOUND ( 'NONE', #5464, .T. ) ;
#7585 = EDGE_LOOP ( 'NONE', ( #8628, #11741, #12983, #11286, #6676, #1957, #10133, #12297, #4036, #9076 ) ) ;
#7586 = CARTESIAN_POINT ( 'NONE',  ( -24.99999999999998934, -100.0000000000065938, -5.046127144261280506 ) ) ;
#7587 = DIRECTION ( 'NONE',  ( -6.158143864569485777E-17, -2.736152283717910599E-16, 1.000000000000000000 ) ) ;
#7588 = LINE ( 'NONE', #10875, #13032 ) ;
#7589 = DIRECTION ( 'NONE',  ( -1.224646799147353207E-16, 1.000000000000000000, 0.000000000000000000 ) ) ;
#7590 = TOROIDAL_SURFACE ( 'NONE', #12321, 71.99999999999998579, 2.000000000000000000 ) ;
#7591 = DIRECTION ( 'NONE',  ( 0.5999999999999989786, -0.8000000000000008216, 0.000000000000000000 ) ) ;
#7592 = ORIENTED_EDGE ( 'NONE', *, *, #4980, .F. ) ;
#7593 = DIRECTION ( 'NONE',  ( 1.000000000000000000, 0.000000000000000000, 0.000000000000000000 ) ) ;
#7594 = ORIENTED_EDGE ( 'NONE', *, *, #6677, .T. ) ;
#7595 = LINE ( 'NONE', #254, #6164 ) ;
#7596 = CIRCLE ( 'NONE', #2909, 16.99999999999998934 ) ;
#7597 = CARTESIAN_POINT ( 'NONE',  ( -8.385254915620294014, 3.280056672672170937, -1.038481780305648437E-15 ) ) ;
#7598 = FACE_BOUND ( 'NONE', #10447, .T. ) ;
#7599 = CARTESIAN_POINT ( 'NONE',  ( -10.69381717166375623, -21.56444287793185666, -1.233455458826524398E-15 ) ) ;
#7600 = DIRECTION ( 'NONE',  ( -0.000000000000000000, -0.000000000000000000, -1.000000000000000000 ) ) ;
#7601 = CARTESIAN_POINT ( 'NONE',  ( 40.05714107113524847, 100.9137399031062898, 2.016203456813714379 ) ) ;
#7602 = DIRECTION ( 'NONE',  ( -6.158143864569485777E-17, -2.736152283717910599E-16, 1.000000000000000000 ) ) ;
#7603 = CIRCLE ( 'NONE', #466, 2.500000000000002220 ) ;
#7604 = CARTESIAN_POINT ( 'NONE',  ( 10.00000000000000711, 139.9999999999999716, -0.5000000000000000000 ) ) ;
#7605 = AXIS2_PLACEMENT_3D ( 'NONE', #194, #4445, #8727 ) ;
#7606 = CARTESIAN_POINT ( 'NONE',  ( -37.50000000000000000, 120.0000000000000142, 2.499999999999999556 ) ) ;
#7607 = VECTOR ( 'NONE', #1425, 1000.000000000000000 ) ;
#7608 = ORIENTED_EDGE ( 'NONE', *, *, #4821, .T. ) ;
#7609 = EDGE_CURVE ( 'NONE', #10258, #6662, #5258, .T. ) ;
#7610 = ORIENTED_EDGE ( 'NONE', *, *, #5303, .F. ) ;
#7611 = TOROIDAL_SURFACE ( 'NONE', #2462, 22.99999999999999289, 2.000000000000000000 ) ;
#7612 = ORIENTED_EDGE ( 'NONE', *, *, #12336, .T. ) ;
#7613 = DIRECTION ( 'NONE',  ( 1.000000000000000000, 9.637352644315596722E-16, 0.000000000000000000 ) ) ;
#7614 = AXIS2_PLACEMENT_3D ( 'NONE', #7670, #3525, #11036 ) ;
#7615 = CARTESIAN_POINT ( 'NONE',  ( -8.385254915620292238, 53.02855864072483882, -1.214179245852635653E-15 ) ) ;
#7616 = DIRECTION ( 'NONE',  ( -6.158143864569485777E-17, -2.736152283717910599E-16, 1.000000000000000000 ) ) ;
#7617 = DIRECTION ( 'NONE',  ( -1.000000000000000000, 0.000000000000000000, 0.000000000000000000 ) ) ;
#7618 = ORIENTED_EDGE ( 'NONE', *, *, #3497, .T. ) ;
#7619 = AXIS2_PLACEMENT_3D ( 'NONE', #12694, #1747, #6305 ) ;
#7620 = EDGE_LOOP ( 'NONE', ( #9867, #920, #7322, #9129 ) ) ;
#7621 = CIRCLE ( 'NONE', #11886, 2.500000000000002220 ) ;
#7622 = EDGE_LOOP ( 'NONE', ( #11114, #5535, #8003, #8944 ) ) ;
#7623 = EDGE_CURVE ( 'NONE', #618, #10695, #2755, .T. ) ;
#7624 = EDGE_CURVE ( 'NONE', #6698, #12375, #13491, .T. ) ;
#7625 = EDGE_CURVE ( 'NONE', #3627, #4145, #5589, .T. ) ;
#7626 = EDGE_LOOP ( 'NONE', ( #9584, #12181 ) ) ;
#7627 = CARTESIAN_POINT ( 'NONE',  ( 22.00000000000000000, 2.694222958124176809E-15, 2.694222958124176809E-15 ) ) ;
#7628 = ORIENTED_EDGE ( 'NONE', *, *, #966, .T. ) ;
#7629 = ADVANCED_FACE ( 'NONE', ( #11578 ), #11205, .T. ) ;
#7630 = FACE_OUTER_BOUND ( 'NONE', #6732, .T. ) ;
#7631 = EDGE_CURVE ( 'NONE', #4855, #9446, #9345, .T. ) ;
#7632 = CYLINDRICAL_SURFACE ( 'NONE', #4200, 9.000000000008999024 ) ;
#7633 = DIRECTION ( 'NONE',  ( 0.000000000000000000, 0.000000000000000000, 1.000000000000000000 ) ) ;
#7634 = VECTOR ( 'NONE', #8168, 1000.000000000000000 ) ;
#7635 = CARTESIAN_POINT ( 'NONE',  ( -34.37593967123855521, 107.8393652239837337, -1.644494279733349718 ) ) ;
#7636 = DIRECTION ( 'NONE',  ( 0.000000000000000000, 1.000000000000000000, 0.000000000000000000 ) ) ;
#7637 = CARTESIAN_POINT ( 'NONE',  ( -7.144831932706865452, -87.96976810164353822, 5.694097463405904058 ) ) ;
#7638 = DIRECTION ( 'NONE',  ( 0.8000000000000024869, 0.5999999999999966471, 0.000000000000000000 ) ) ;
#7639 = ORIENTED_EDGE ( 'NONE', *, *, #979, .F. ) ;
#7640 = ORIENTED_EDGE ( 'NONE', *, *, #1161, .F. ) ;
#7641 = ORIENTED_EDGE ( 'NONE', *, *, #12004, .F. ) ;
#7642 = ADVANCED_FACE ( 'NONE', ( #7298 ), #9609, .F. ) ;
#7643 = PRESENTATION_LAYER_ASSIGNMENT (  '', '', ( #10127 ) ) ;
#7644 = LINE ( 'NONE', #7572, #9831 ) ;
#7645 = DIRECTION ( 'NONE',  ( -6.158143864569485777E-17, -2.736152283717910599E-16, 1.000000000000000000 ) ) ;
#7646 = ORIENTED_EDGE ( 'NONE', *, *, #10066, .T. ) ;
#7647 = CARTESIAN_POINT ( 'NONE',  ( 0.000000000000000000, 71.01020514433645303, 0.5000000000000000000 ) ) ;
#7648 = SURFACE_STYLE_USAGE ( .BOTH. , #13000 ) ;
#7649 = CARTESIAN_POINT ( 'NONE',  ( 8.385254915620292238, 59.82872437272870769, 9.722760835075757558E-16 ) ) ;
#7650 = EDGE_CURVE ( 'NONE', #10190, #297, #10745, .T. ) ;
#7651 = CARTESIAN_POINT ( 'NONE',  ( 10.69381717166375800, 6.709890972096426154, -21.38763434332750890 ) ) ;
#7652 = DIRECTION ( 'NONE',  ( -6.158143864569485777E-17, -2.736152283717910599E-16, 1.000000000000000000 ) ) ;
#7653 = CARTESIAN_POINT ( 'NONE',  ( 8.385254915620292238, 90.00000000000000000, 8.679704431140114636E-16 ) ) ;
#7654 = CARTESIAN_POINT ( 'NONE',  ( 8.385254915620288685, 43.60378069071538221, 9.522168693316292075E-16 ) ) ;
#7655 = CARTESIAN_POINT ( 'NONE',  ( -2.010743657263654653E-15, 71.87811454074363837, -1.269264606320675724E-16 ) ) ;
#7656 = DIRECTION ( 'NONE',  ( 0.9960067511297464593, -0.08927794634716622324, 3.401418580343279473E-17 ) ) ;
#7657 = ORIENTED_EDGE ( 'NONE', *, *, #7372, .T. ) ;
#7658 = DIRECTION ( 'NONE',  ( -2.797435172181481150E-17, 1.000000000000000000, -1.765856845898762549E-18 ) ) ;
#7659 = CARTESIAN_POINT ( 'NONE',  ( 53.14943414785363984, 10.84564612680554241, -2.499999999999994671 ) ) ;
#7660 = ORIENTED_EDGE ( 'NONE', *, *, #7455, .F. ) ;
#7661 = LINE ( 'NONE', #4573, #8609 ) ;
#7662 = CARTESIAN_POINT ( 'NONE',  ( -6.999999999999999112, -20.00000000000000355, 7.500000000000000000 ) ) ;
#7663 = ORIENTED_EDGE ( 'NONE', *, *, #12190, .F. ) ;
#7664 = CIRCLE ( 'NONE', #12163, 12.49999999999998757 ) ;
#7665 = CARTESIAN_POINT ( 'NONE',  ( -10.69381717166375623, 6.709890972096426154, -1.333312310811123490E-15 ) ) ;
#7666 = VERTEX_POINT ( 'NONE', #5326 ) ;
#7667 = CARTESIAN_POINT ( 'NONE',  ( 35.08961652778860696, 18.74878582411816197, -2.499999999999993783 ) ) ;
#7668 = DIRECTION ( 'NONE',  ( -2.797435172181481150E-17, 1.000000000000000000, -1.765856845898762549E-18 ) ) ;
#7669 = DIRECTION ( 'NONE',  ( 1.000000000000000000, 0.000000000000000000, 0.000000000000000000 ) ) ;
#7670 = CARTESIAN_POINT ( 'NONE',  ( -29.00000000000000000, 123.0000000000000142, -2.499999999999999556 ) ) ;
#7671 = CARTESIAN_POINT ( 'NONE',  ( 10.69381717166375800, 25.55944687211528787, -21.38763434332750890 ) ) ;
#7672 = DIRECTION ( 'NONE',  ( -2.797435172181481150E-17, 1.000000000000000000, -1.765856845898762549E-18 ) ) ;
#7673 = FACE_OUTER_BOUND ( 'NONE', #7620, .T. ) ;
#7674 = CARTESIAN_POINT ( 'NONE',  ( -15.29705854078138927, 17.78624592198638155, -1.936165306082118094E-15 ) ) ;
#7675 = VERTEX_POINT ( 'NONE', #11842 ) ;
#7676 = AXIS2_PLACEMENT_3D ( 'NONE', #6119, #1902, #7426 ) ;
#7677 = ORIENTED_EDGE ( 'NONE', *, *, #9461, .F. ) ;
#7678 = CARTESIAN_POINT ( 'NONE',  ( 15.29705854078138749, 47.94714734142005597, 1.790347283588440388E-15 ) ) ;
#7679 = DIRECTION ( 'NONE',  ( 1.000000000000000000, 0.000000000000000000, 0.000000000000000000 ) ) ;
#7680 = VERTEX_POINT ( 'NONE', #6652 ) ;
#7681 = CARTESIAN_POINT ( 'NONE',  ( -12.99579180576517068, 26.38439787695498495, -1.684707622963446858E-15 ) ) ;
#7682 = DIRECTION ( 'NONE',  ( -6.158143864569485777E-17, -2.736152283717910599E-16, 1.000000000000000000 ) ) ;
#7683 = DIRECTION ( 'NONE',  ( 1.000000000000000000, 0.000000000000000000, -0.000000000000000000 ) ) ;
#7684 = EDGE_CURVE ( 'NONE', #6329, #7425, #8298, .T. ) ;
#7685 = UNCERTAINTY_MEASURE_WITH_UNIT (LENGTH_MEASURE( 1.000000000000000082E-05 ), #8533, 'distance_accuracy_value', 'NONE');
#7686 = LINE ( 'NONE', #10773, #2419 ) ;
#7687 = CIRCLE ( 'NONE', #11510, 25.50000000002550138 ) ;
#7688 = EDGE_LOOP ( 'NONE', ( #3997, #9985, #4627, #11062 ) ) ;
#7689 = ORIENTED_EDGE ( 'NONE', *, *, #1948, .T. ) ;
#7690 = VERTEX_POINT ( 'NONE', #3218 ) ;
#7691 = ORIENTED_EDGE ( 'NONE', *, *, #7211, .T. ) ;
#7692 = CARTESIAN_POINT ( 'NONE',  ( 1.958204620527036102E-15, -69.99999999999998579, 1.236099792129133461E-16 ) ) ;
#7693 = VERTEX_POINT ( 'NONE', #10913 ) ;
#7694 = CARTESIAN_POINT ( 'NONE',  ( -10.69381717166375800, 72.68333662216240043, 21.38763434332750535 ) ) ;
#7695 = MANIFOLD_SOLID_BREP ( 'Join1', #10288 ) ;
#7696 = LINE ( 'NONE', #11979, #6673 ) ;
#7697 = DIRECTION ( 'NONE',  ( 0.000000000000000000, -1.000000000000000000, 0.000000000000000000 ) ) ;
#7698 = CARTESIAN_POINT ( 'NONE',  ( -25.00000000000000355, 120.0000000000000142, 2.499999999999999556 ) ) ;
#7699 = CARTESIAN_POINT ( 'NONE',  ( 2.482863863605449417, 90.00000000000002842, -4.353049703108322177 ) ) ;
#7700 = ADVANCED_FACE ( 'NONE', ( #1318, #9887 ), #11980, .T. ) ;
#7701 = CARTESIAN_POINT ( 'NONE',  ( 12.99579180576518134, -30.16426982310158422, -25.99158361153034491 ) ) ;
#7702 = CARTESIAN_POINT ( 'NONE',  ( 39.06230589874905235, 109.5835921350012825, -7.500000000000000000 ) ) ;
#7703 = ADVANCED_FACE ( 'NONE', ( #6385 ), #7611, .T. ) ;
#7704 = VECTOR ( 'NONE', #5656, 999.9999999999998863 ) ;
#7705 = ORIENTED_EDGE ( 'NONE', *, *, #12778, .F. ) ;
#7706 = EDGE_CURVE ( 'NONE', #7751, #6696, #9424, .T. ) ;
#7707 = EDGE_CURVE ( 'NONE', #6483, #9883, #12798, .T. ) ;
#7708 = TOROIDAL_SURFACE ( 'NONE', #5254, 22.49999999999998934, 5.000000000000000000 ) ;
#7709 = CYLINDRICAL_SURFACE ( 'NONE', #4446, 2.000000000000001776 ) ;
#7710 = CARTESIAN_POINT ( 'NONE',  ( 16.34455450841069890, -1.870656171256065425, -2.500000000000000888 ) ) ;
#7711 = ORIENTED_EDGE ( 'NONE', *, *, #7281, .F. ) ;
#7712 = FACE_OUTER_BOUND ( 'NONE', #846, .T. ) ;
#7713 = DIRECTION ( 'NONE',  ( -6.158143864569485777E-17, -2.736152283717910599E-16, 1.000000000000000000 ) ) ;
#7714 = CARTESIAN_POINT ( 'NONE',  ( -15.29705854078139105, 8.361467971976955127, -3.761435144035948792E-15 ) ) ;
#7715 = LINE ( 'NONE', #11997, #2051 ) ;
#7716 = AXIS2_PLACEMENT_3D ( 'NONE', #1481, #10041, #8318 ) ;
#7717 = CYLINDRICAL_SURFACE ( 'NONE', #1121, 25.00000000000000355 ) ;
#7718 = CARTESIAN_POINT ( 'NONE',  ( 15.29705854078138572, 90.00000000000000000, 1.714422261702872371E-15 ) ) ;
#7719 = CARTESIAN_POINT ( 'NONE',  ( -21.99999999999999289, -97.00000000000000000, 7.500000000000000000 ) ) ;
#7720 = CARTESIAN_POINT ( 'NONE',  ( -15.29705854078139637, 90.00000000000000000, -1.589271161308885878E-16 ) ) ;
#7721 = CIRCLE ( 'NONE', #9529, 25.50000000002549783 ) ;
#7722 = EDGE_LOOP ( 'NONE', ( #4062, #13596, #9405, #13337 ) ) ;
#7723 = VERTEX_POINT ( 'NONE', #7765 ) ;
#7724 = EDGE_CURVE ( 'NONE', #3535, #6779, #12051, .T. ) ;
#7725 = ORIENTED_EDGE ( 'NONE', *, *, #12353, .F. ) ;
#7726 = AXIS2_PLACEMENT_3D ( 'NONE', #10185, #453, #4859 ) ;
#7727 = CARTESIAN_POINT ( 'NONE',  ( -24.99999999999998579, -99.51472204732199600, -3.411167378945827000 ) ) ;
#7728 = AXIS2_PLACEMENT_3D ( 'NONE', #12064, #12864, #2176 ) ;
#7729 = FACE_OUTER_BOUND ( 'NONE', #12848, .T. ) ;
#7730 = EDGE_LOOP ( 'NONE', ( #13457, #3095, #10484 ) ) ;
#7731 = CARTESIAN_POINT ( 'NONE',  ( 12.99553232110414669, -17.19957910547634228, 0.000000000000000000 ) ) ;
#7732 = ORIENTED_EDGE ( 'NONE', *, *, #9894, .T. ) ;
#7733 = CIRCLE ( 'NONE', #4381, 24.99999999999998934 ) ;
#7734 = CARTESIAN_POINT ( 'NONE',  ( -24.37649275748776390, -100.0000000000000000, -7.500000000000000000 ) ) ;
#7735 = CARTESIAN_POINT ( 'NONE',  ( -8.385254915620295790, 24.75422479069652582, -1.114322393868036955E-15 ) ) ;
#7736 = CARTESIAN_POINT ( 'NONE',  ( -8.385254915620286909, 43.60378069071538221, -16.77050983124057737 ) ) ;
#7737 = DIRECTION ( 'NONE',  ( 1.000000000000000000, 0.000000000000000000, -0.000000000000000000 ) ) ;
#7738 = CARTESIAN_POINT ( 'NONE',  ( 10.00000000000000000, 97.99999999999994316, -2.500000000000000000 ) ) ;
#7739 = DIRECTION ( 'NONE',  ( 1.000000000000000000, 0.000000000000000000, 0.000000000000000000 ) ) ;
#7740 = CIRCLE ( 'NONE', #3260, 25.50000000002549783 ) ;
#7741 = CARTESIAN_POINT ( 'NONE',  ( -8.385254915620297567, 78.67828027274755698, -1.389345798431728350E-16 ) ) ;
#7742 = DIRECTION ( 'NONE',  ( -6.158143864569485777E-17, -2.736152283717910599E-16, 1.000000000000000000 ) ) ;
#7743 = ADVANCED_FACE ( 'NONE', ( #10024 ), #9956, .T. ) ;
#7744 = VERTEX_POINT ( 'NONE', #1611 ) ;
#7745 = ORIENTED_EDGE ( 'NONE', *, *, #517, .T. ) ;
#7746 = CARTESIAN_POINT ( 'NONE',  ( 37.50000000000000711, 4.592425496802575156E-15, -4.000000000000000000 ) ) ;
#7747 = AXIS2_PLACEMENT_3D ( 'NONE', #12097, #1506, #10064 ) ;
#7748 = ORIENTED_EDGE ( 'NONE', *, *, #6532, .T. ) ;
#7749 = CYLINDRICAL_SURFACE ( 'NONE', #2563, 15.29705854078138749 ) ;
#7750 = APPLICATION_PROTOCOL_DEFINITION ( 'draft international standard', 'automotive_design', 1998, #6476 ) ;
#7751 = VERTEX_POINT ( 'NONE', #7007 ) ;
#7752 = DIRECTION ( 'NONE',  ( -1.000000000000000000, 0.000000000000000000, 0.000000000000000000 ) ) ;
#7753 = CARTESIAN_POINT ( 'NONE',  ( 13.94188849117746010, 1.893657697999893808, -2.500000000000000000 ) ) ;
#7754 = FACE_OUTER_BOUND ( 'NONE', #7759, .T. ) ;
#7755 = DIRECTION ( 'NONE',  ( -0.5999999999999989786, -0.8000000000000008216, 0.000000000000000000 ) ) ;
#7756 = ORIENTED_EDGE ( 'NONE', *, *, #2310, .F. ) ;
#7757 = CARTESIAN_POINT ( 'NONE',  ( -8.385254915620294014, -24.99427717735608212, -2.007341458301378282E-15 ) ) ;
#7758 = EDGE_CURVE ( 'NONE', #5016, #13646, #3916, .T. ) ;
#7759 = EDGE_LOOP ( 'NONE', ( #253, #9146, #3280, #1004 ) ) ;
#7760 = ORIENTED_EDGE ( 'NONE', *, *, #9201, .T. ) ;
#7761 = DIRECTION ( 'NONE',  ( -2.797435172181481150E-17, 1.000000000000000000, -1.765856845898762549E-18 ) ) ;
#7762 = VERTEX_POINT ( 'NONE', #13435 ) ;
#7763 = CARTESIAN_POINT ( 'NONE',  ( 22.00000000000001066, -97.00000000000000000, 0.000000000000000000 ) ) ;
#7764 = CYLINDRICAL_SURFACE ( 'NONE', #12514, 25.50000000002549783 ) ;
#7765 = CARTESIAN_POINT ( 'NONE',  ( 53.02537423504344360, -5.158573900538658386, 2.499999999999999556 ) ) ;
#7766 = FACE_OUTER_BOUND ( 'NONE', #3401, .T. ) ;
#7767 = LINE ( 'NONE', #12054, #7453 ) ;
#7768 = CARTESIAN_POINT ( 'NONE',  ( 10.69381717166376511, -30.98922082794128485, -21.38763434332751956 ) ) ;
#7769 = LINE ( 'NONE', #9892, #13140 ) ;
#7770 = ORIENTED_EDGE ( 'NONE', *, *, #3425, .T. ) ;
#7771 = ORIENTED_EDGE ( 'NONE', *, *, #5225, .T. ) ;
#7772 = CARTESIAN_POINT ( 'NONE',  ( 0.6173387890061948768, -40.00941361824966691, -4.961742921553712549 ) ) ;
#7773 = EDGE_CURVE ( 'NONE', #9005, #397, #6938, .T. ) ;
#7774 = CARTESIAN_POINT ( 'NONE',  ( -3.521437233922030785, 90.23421079890158580, 3.553194557407191922 ) ) ;
#7775 = EDGE_CURVE ( 'NONE', #4007, #13581, #4246, .T. ) ;
#7776 = LINE ( 'NONE', #5685, #11421 ) ;
#7777 = VERTEX_POINT ( 'NONE', #13128 ) ;
#7778 = CARTESIAN_POINT ( 'NONE',  ( 8.385254915620292238, -3.520109059331755219, 2.053795118489800004E-15 ) ) ;
#7779 = FILL_AREA_STYLE_COLOUR ( '', #7503 ) ;
#7780 = AXIS2_PLACEMENT_3D ( 'NONE', #1317, #5598, #8753 ) ;
#7781 = CARTESIAN_POINT ( 'NONE',  ( 0.1852016367020528076, -70.00000000000000000, -1.488522876466090272 ) ) ;
#7782 = CARTESIAN_POINT ( 'NONE',  ( -2.557893175568157318, -128.7272727272848272, 3.337007314118914714 ) ) ;
#7783 = DIRECTION ( 'NONE',  ( -0.000000000000000000, -0.000000000000000000, -1.000000000000000000 ) ) ;
#7784 = EDGE_CURVE ( 'NONE', #8545, #8344, #6087, .T. ) ;
#7785 = LINE ( 'NONE', #9762, #4 ) ;
#7786 = DIRECTION ( 'NONE',  ( 0.000000000000000000, 1.000000000000000000, 0.000000000000000000 ) ) ;
#7787 = CARTESIAN_POINT ( 'NONE',  ( 36.36363636363638108, 142.2680885707561629, -0.5000000000000000000 ) ) ;
#7788 = CARTESIAN_POINT ( 'NONE',  ( 0.000000000000000000, -20.00000000000000000, 0.000000000000000000 ) ) ;
#7789 = VECTOR ( 'NONE', #3137, 1000.000000000000000 ) ;
#7790 = ORIENTED_EDGE ( 'NONE', *, *, #7151, .T. ) ;
#7791 = CIRCLE ( 'NONE', #1535, 9.000000000008999024 ) ;
#7792 = DIRECTION ( 'NONE',  ( -6.158143864569485777E-17, -2.736152283717910599E-16, 1.000000000000000000 ) ) ;
#7793 = CARTESIAN_POINT ( 'NONE',  ( -2.339066459587731637E-16, 8.361467971976981772, -1.476515546007874940E-17 ) ) ;
#7794 = EDGE_CURVE ( 'NONE', #13136, #7032, #13284, .T. ) ;
#7795 = CARTESIAN_POINT ( 'NONE',  ( -10.00000000000000711, 139.9999999999999716, -0.5000000000000000000 ) ) ;
#7796 = EDGE_CURVE ( 'NONE', #3488, #8612, #6800, .T. ) ;
#7797 = PLANE ( 'NONE',  #12337 ) ;
#7798 = ORIENTED_EDGE ( 'NONE', *, *, #12372, .F. ) ;
#7799 = ORIENTED_EDGE ( 'NONE', *, *, #2071, .F. ) ;
#7800 = DIRECTION ( 'NONE',  ( -0.6000000000000001998, 0.7999999999999998224, 0.000000000000000000 ) ) ;
#7801 = ORIENTED_EDGE ( 'NONE', *, *, #4212, .T. ) ;
#7802 = DIRECTION ( 'NONE',  ( -6.158143864569485777E-17, -2.736152283717910599E-16, 1.000000000000000000 ) ) ;
#7803 = CIRCLE ( 'NONE', #442, 9.000000000008999024 ) ;
#7804 = CARTESIAN_POINT ( 'NONE',  ( -37.50000000000000711, -4.286263797015736496E-15, -7.500000000000000000 ) ) ;
#7805 = EDGE_CURVE ( 'NONE', #1833, #9552, #6064, .T. ) ;
#7806 = PLANE ( 'NONE',  #2224 ) ;
#7807 = EDGE_CURVE ( 'NONE', #3663, #3080, #9855, .T. ) ;
#7808 = VECTOR ( 'NONE', #3820, 1000.000000000000000 ) ;
#7809 = CARTESIAN_POINT ( 'NONE',  ( 0.000000000000000000, 71.01020514433645303, -2.500000000000000000 ) ) ;
#7810 = FACE_OUTER_BOUND ( 'NONE', #6480, .T. ) ;
#7811 = CARTESIAN_POINT ( 'NONE',  ( -20.00023673640403743, 26.72039747452867076, -1.279702169315401150 ) ) ;
#7812 = FACE_OUTER_BOUND ( 'NONE', #5916, .T. ) ;
#7813 = CARTESIAN_POINT ( 'NONE',  ( -2.517691654963332357E-15, 90.00000000000000000, -1.589271161308885878E-16 ) ) ;
#7814 = CARTESIAN_POINT ( 'NONE',  ( 8.385254915620299343, -6.144721277337255039, -16.77050983124059158 ) ) ;
#7815 = EDGE_LOOP ( 'NONE', ( #9387, #8829, #11296, #6201 ) ) ;
#7816 = DIRECTION ( 'NONE',  ( -1.000000000000000000, 0.000000000000000000, 0.000000000000000000 ) ) ;
#7817 = VECTOR ( 'NONE', #9688, 1000.000000000000000 ) ;
#7818 = ORIENTED_EDGE ( 'NONE', *, *, #12271, .T. ) ;
#7819 = AXIS2_PLACEMENT_3D ( 'NONE', #4029, #8316, #6219 ) ;
#7820 = EDGE_CURVE ( 'NONE', #13581, #4007, #3811, .T. ) ;
#7821 = ORIENTED_EDGE ( 'NONE', *, *, #7396, .T. ) ;
#7822 = CARTESIAN_POINT ( 'NONE',  ( 9.628507540654561270E-16, -34.41905512736551032, 6.077912412602530076E-17 ) ) ;
#7823 = ORIENTED_EDGE ( 'NONE', *, *, #8419, .T. ) ;
#7824 = DIRECTION ( 'NONE',  ( -2.797435172181481150E-17, 1.000000000000000000, -1.765856845898762549E-18 ) ) ;
#7825 = EDGE_CURVE ( 'NONE', #12409, #9553, #11221, .T. ) ;
#7826 = CIRCLE ( 'NONE', #11859, 17.49999999999999645 ) ;
#7827 = CARTESIAN_POINT ( 'NONE',  ( 8.894289287455980914E-16, -31.79444290936001138, 5.614443467303076398E-17 ) ) ;
#7828 = LINE ( 'NONE', #6783, #1721 ) ;
#7829 = CIRCLE ( 'NONE', #1788, 8.385254915620297567 ) ;
#7830 = DIRECTION ( 'NONE',  ( 0.000000000000000000, 0.000000000000000000, 1.000000000000000000 ) ) ;
#7831 = VECTOR ( 'NONE', #6680, 1000.000000000000000 ) ;
#7832 = UNCERTAINTY_MEASURE_WITH_UNIT (LENGTH_MEASURE( 1.000000000000000082E-05 ), #6812, 'distance_accuracy_value', 'NONE');
#7833 = CARTESIAN_POINT ( 'NONE',  ( 9.723082553384461590, -72.03366436399431905, 2.708544018860256308 ) ) ;
#7834 = ORIENTED_EDGE ( 'NONE', *, *, #9693, .T. ) ;
#7835 = FACE_OUTER_BOUND ( 'NONE', #1688, .T. ) ;
#7836 = EDGE_LOOP ( 'NONE', ( #11817, #10242, #10340, #12511 ) ) ;
#7837 = AXIS2_PLACEMENT_3D ( 'NONE', #6122, #10394, #790 ) ;
#7838 = CARTESIAN_POINT ( 'NONE',  ( 1.084353620409068652E-15, -38.76242177807012723, 6.844888786042043893E-17 ) ) ;
#7839 = AXIS2_PLACEMENT_3D ( 'NONE', #11095, #10345, #12727 ) ;
#7840 = CIRCLE ( 'NONE', #6957, 2.000000000000000000 ) ;
#7841 = ORIENTED_EDGE ( 'NONE', *, *, #6497, .T. ) ;
#7842 = VERTEX_POINT ( 'NONE', #3849 ) ;
#7843 = CARTESIAN_POINT ( 'NONE',  ( -60.00000000000001421, 20.00000000000000000, 4.000000000000000000 ) ) ;
#7844 = CARTESIAN_POINT ( 'NONE',  ( 15.29705854078138216, 76.22148119144830503, 30.59411708156277854 ) ) ;
#7845 = CARTESIAN_POINT ( 'NONE',  ( 0.000000000000000000, 40.00000000000000000, 0.000000000000000000 ) ) ;
#7846 = CARTESIAN_POINT ( 'NONE',  ( -10.00000000000000711, 92.00000000000000000, -2.500000000000000000 ) ) ;
#7847 = CARTESIAN_POINT ( 'NONE',  ( -2.008006351130390499, -80.00378950643924725, -9.910921267331605833 ) ) ;
#7848 = VECTOR ( 'NONE', #7113, 1000.000000000000000 ) ;
#7849 = ADVANCED_FACE ( 'NONE', ( #13640 ), #12416, .T. ) ;
#7850 = DIRECTION ( 'NONE',  ( -6.158143864569485777E-17, -2.736152283717910599E-16, 1.000000000000000000 ) ) ;
#7851 = ORIENTED_EDGE ( 'NONE', *, *, #2158, .T. ) ;
#7852 = AXIS2_PLACEMENT_3D ( 'NONE', #8900, #3779, #12203 ) ;
#7853 = CIRCLE ( 'NONE', #7188, 15.29705854078139105 ) ;
#7854 = ORIENTED_EDGE ( 'NONE', *, *, #7040, .F. ) ;
#7855 = VERTEX_POINT ( 'NONE', #8339 ) ;
#7856 = CARTESIAN_POINT ( 'NONE',  ( 35.22727272727274084, 140.0412797136805523, -7.500000000000000000 ) ) ;
#7857 = CARTESIAN_POINT ( 'NONE',  ( 8.804495088766337574, -73.18181818181338372, 4.925729831870250486 ) ) ;
#7858 = ORIENTED_EDGE ( 'NONE', *, *, #7290, .F. ) ;
#7859 = CARTESIAN_POINT ( 'NONE',  ( 4.804172150869134406, 90.20479154739604155, 1.391179344134541473 ) ) ;
#7860 =( LENGTH_UNIT ( ) NAMED_UNIT ( * ) SI_UNIT ( .MILLI., .METRE. ) );
#7861 = DIRECTION ( 'NONE',  ( 1.000000000000000000, 0.000000000000000000, 0.000000000000000000 ) ) ;
#7862 = CIRCLE ( 'NONE', #6086, 4.999999999999998224 ) ;
#7863 = CARTESIAN_POINT ( 'NONE',  ( -28.15981099771517648, -27.70535714287384366, 7.500000000000000000 ) ) ;
#7864 = CIRCLE ( 'NONE', #3608, 9.000000000008999024 ) ;
#7865 = CARTESIAN_POINT ( 'NONE',  ( 4.547999443521274721, -70.00000000000000000, 2.077426547854386296 ) ) ;
#7866 = FACE_OUTER_BOUND ( 'NONE', #5854, .T. ) ;
#7867 = CARTESIAN_POINT ( 'NONE',  ( 0.05313321603437554802, -142.5800865800495671, 3.258060136338194468 ) ) ;
#7868 = DIRECTION ( 'NONE',  ( -0.000000000000000000, -0.000000000000000000, -1.000000000000000000 ) ) ;
#7869 = CARTESIAN_POINT ( 'NONE',  ( 42.16244658108817589, 105.4500712252157655, -2.499999999999999556 ) ) ;
#7870 = DIRECTION ( 'NONE',  ( 2.797435172181480534E-17, -1.000000000000000000, 1.765856845898762164E-18 ) ) ;
#7871 = ORIENTED_EDGE ( 'NONE', *, *, #11677, .F. ) ;
#7872 = EDGE_LOOP ( 'NONE', ( #2714, #5266, #2878, #3926 ) ) ;
#7873 = EDGE_CURVE ( 'NONE', #11146, #11917, #10574, .T. ) ;
#7874 = VERTEX_POINT ( 'NONE', #7145 ) ;
#7875 = CARTESIAN_POINT ( 'NONE',  ( -8.385254915620295790, 90.00000000000000000, -1.589271161308885878E-16 ) ) ;
#7876 = ORIENTED_EDGE ( 'NONE', *, *, #2597, .T. ) ;
#7877 = TOROIDAL_SURFACE ( 'NONE', #8334, 22.99999999999999289, 2.000000000000000000 ) ;
#7878 = DIRECTION ( 'NONE',  ( -6.158143864569485777E-17, -2.736152283717910599E-16, 1.000000000000000000 ) ) ;
#7879 = CYLINDRICAL_SURFACE ( 'NONE', #4034, 25.50000000002549783 ) ;
#7880 = LINE ( 'NONE', #1773, #6181 ) ;
#7881 = CARTESIAN_POINT ( 'NONE',  ( 7.000000000000007994, -35.00000000000000000, 7.500000000000000000 ) ) ;
#7882 = VERTEX_POINT ( 'NONE', #9183 ) ;
#7883 = DIRECTION ( 'NONE',  ( -0.9923485843107423543, -2.797833471351478217E-17, -0.1234677578012386562 ) ) ;
#7884 = ORIENTED_EDGE ( 'NONE', *, *, #2697, .F. ) ;
#7885 = DIRECTION ( 'NONE',  ( 1.000000000000000000, 0.000000000000000000, 0.000000000000000000 ) ) ;
#7886 = DIRECTION ( 'NONE',  ( -2.797435172181481150E-17, 1.000000000000000000, -1.765856845898762549E-18 ) ) ;
#7887 = CARTESIAN_POINT ( 'NONE',  ( 8.385254915620292238, 22.12961257269105531, 1.008767855514154504E-15 ) ) ;
#7888 = B_SPLINE_CURVE_WITH_KNOTS ( 'NONE', 3,
 ( #7131, #11408, #4045, #4109 ),
 .UNSPECIFIED., .F., .F.,
 ( 4, 4 ),
 ( 0.000000000000000000, 1.000000000000000000 ),
 .UNSPECIFIED. ) ;
#7889 = CARTESIAN_POINT ( 'NONE',  ( 41.99999999999999289, 120.0000000000000142, 0.5000000000000000000 ) ) ;
#7890 = CARTESIAN_POINT ( 'NONE',  ( -8.385254915620295790, 69.25350232273815720, -1.222917711790730109E-16 ) ) ;
#7891 = CARTESIAN_POINT ( 'NONE',  ( -2.595029975318955628, -79.59366873198513304, -9.795567015018859180 ) ) ;
#7892 = CARTESIAN_POINT ( 'NONE',  ( 10.69381717166375267, 63.25855867215299355, 2.619229793989003951E-15 ) ) ;
#7893 = DIRECTION ( 'NONE',  ( 0.000000000000000000, 0.000000000000000000, 1.000000000000000000 ) ) ;
#7894 = EDGE_CURVE ( 'NONE', #7680, #2431, #11494, .T. ) ;
#7895 = DIRECTION ( 'NONE',  ( 0.08715574274765883200, -0.9961946980917454342, -0.000000000000000000 ) ) ;
#7896 = EDGE_CURVE ( 'NONE', #12324, #4849, #11275, .T. ) ;
#7897 = DIRECTION ( 'NONE',  ( -1.000000000000000000, 0.000000000000000000, 0.000000000000000000 ) ) ;
#7898 = VERTEX_POINT ( 'NONE', #9325 ) ;
#7899 = FACE_OUTER_BOUND ( 'NONE', #11970, .T. ) ;
#7900 = EDGE_CURVE ( 'NONE', #5991, #5794, #8972, .T. ) ;
#7901 = EDGE_CURVE ( 'NONE', #6530, #7206, #4709, .T. ) ;
#7902 = ORIENTED_EDGE ( 'NONE', *, *, #12884, .T. ) ;
#7903 = DIRECTION ( 'NONE',  ( 1.000000000000000000, 0.000000000000000000, 0.000000000000000000 ) ) ;
#7904 = SHAPE_DEFINITION_REPRESENTATION ( #8005, #1365 ) ;
#7905 = ORIENTED_EDGE ( 'NONE', *, *, #8075, .T. ) ;
#7906 = DIRECTION ( 'NONE',  ( -2.797435172181481150E-17, 1.000000000000000000, -1.765856845898762549E-18 ) ) ;
#7907 = CIRCLE ( 'NONE', #971, 25.50000000002549783 ) ;
#7908 = CARTESIAN_POINT ( 'NONE',  ( -15.29705854078138749, 38.52236939141059935, -6.802498971006334016E-17 ) ) ;
#7909 = AXIS2_PLACEMENT_3D ( 'NONE', #2010, #11481, #12684 ) ;
#7910 = CARTESIAN_POINT ( 'NONE',  ( -8.385254915620295790, 22.12961257269105531, 16.77050983124058448 ) ) ;
#7911 = EDGE_CURVE ( 'NONE', #11359, #12557, #482, .T. ) ;
#7912 = DIRECTION ( 'NONE',  ( 0.000000000000000000, 0.000000000000000000, 1.000000000000000000 ) ) ;
#7913 = ORIENTED_EDGE ( 'NONE', *, *, #1639, .F. ) ;
#7914 = TOROIDAL_SURFACE ( 'NONE', #12850, 71.99999999999998579, 2.000000000000000000 ) ;
#7915 = DIRECTION ( 'NONE',  ( 0.000000000000000000, 0.000000000000000000, 1.000000000000000000 ) ) ;
#7916 = ORIENTED_EDGE ( 'NONE', *, *, #10213, .F. ) ;
#7917 = ADVANCED_FACE ( 'NONE', ( #8204 ), #6511, .F. ) ;
#7918 = AXIS2_PLACEMENT_3D ( 'NONE', #13212, #10917, #220 ) ;
#7919 = CARTESIAN_POINT ( 'NONE',  ( 12.99553232110414669, -26.62435705548577047, 1.656305067313535556E-15 ) ) ;
#7920 = ORIENTED_EDGE ( 'NONE', *, *, #13254, .F. ) ;
#7921 = ORIENTED_EDGE ( 'NONE', *, *, #707, .F. ) ;
#7922 = DIRECTION ( 'NONE',  ( -0.000000000000000000, -0.000000000000000000, -1.000000000000000000 ) ) ;
#7923 = CARTESIAN_POINT ( 'NONE',  ( -12.99553232110414491, -7.774801155466915858, -1.564035334333850472E-15 ) ) ;
#7924 = AXIS2_PLACEMENT_3D ( 'NONE', #2324, #6607, #1276 ) ;
#7925 = DIRECTION ( 'NONE',  ( -0.6466635011015237078, -0.7627754036039179342, -0.000000000000000000 ) ) ;
#7926 = CARTESIAN_POINT ( 'NONE',  ( 35.00000000000001421, -135.0000000000000000, 4.286263797015737285E-15 ) ) ;
#7927 = CARTESIAN_POINT ( 'NONE',  ( 7.162946923110105502, -96.44493861733469942, 3.807625378222109003 ) ) ;
#7928 = CARTESIAN_POINT ( 'NONE',  ( -8.385254915620288685, 15.32944684068712782, -16.77050983124058448 ) ) ;
#7929 = EDGE_LOOP ( 'NONE', ( #9542, #797, #12232, #1117 ) ) ;
#7930 = B_SPLINE_CURVE_WITH_KNOTS ( 'NONE', 3,
 ( #8710, #3515, #7727, #11024, #5629, #2268, #1285, #12947 ),
 .UNSPECIFIED., .F., .F.,
 ( 4, 2, 2, 4 ),
 ( 0.02189346042269429971, 0.02442701477284284911, 0.02569379194791712034, 0.02696056912299139158 ),
 .UNSPECIFIED. ) ;
#7931 = VERTEX_POINT ( 'NONE', #6236 ) ;
#7932 = ADVANCED_FACE ( 'NONE', ( #1885 ), #7105, .T. ) ;
#7933 = AXIS2_PLACEMENT_3D ( 'NONE', #7086, #377, #10111 ) ;
#7934 = EDGE_LOOP ( 'NONE', ( #4553, #6643, #10304, #336 ) ) ;
#7935 = CARTESIAN_POINT ( 'NONE',  ( 0.000000000000000000, 71.01020514433645303, 2.500000000000000000 ) ) ;
#7936 = CARTESIAN_POINT ( 'NONE',  ( 9.940250983052006717, -69.87878787878412368, 1.425521750854503722 ) ) ;
#7937 = ORIENTED_EDGE ( 'NONE', *, *, #7894, .T. ) ;
#7938 = CARTESIAN_POINT ( 'NONE',  ( 4.895853646792283520, 90.06529264441493865, 1.023585852534436347 ) ) ;
#7939 = LINE ( 'NONE', #11090, #4001 ) ;
#7940 = CARTESIAN_POINT ( 'NONE',  ( 15.29705854078139637, -18.02629830864593785, 1.919277763901059081E-15 ) ) ;
#7941 = CARTESIAN_POINT ( 'NONE',  ( 0.3728392436379902586, -81.93939393934687132, -10.00978956350897064 ) ) ;
#7942 = CARTESIAN_POINT ( 'NONE',  ( -8.385254915620297567, 78.67828027274755698, -1.389345798431728350E-16 ) ) ;
#7943 = AXIS2_PLACEMENT_3D ( 'NONE', #5727, #7824, #2578 ) ;
#7944 = CARTESIAN_POINT ( 'NONE',  ( 15.34996685542352424, -16.25414556851945491, 3.363331797608928309 ) ) ;
#7945 = CARTESIAN_POINT ( 'NONE',  ( -10.00000000000000711, 139.9999999999999716, -2.500000000000000000 ) ) ;
#7946 = AXIS2_PLACEMENT_3D ( 'NONE', #11879, #9920, #4659 ) ;
#7947 = ORIENTED_EDGE ( 'NONE', *, *, #3429, .T. ) ;
#7948 = CIRCLE ( 'NONE', #8865, 8.385254915620294014 ) ;
#7949 = ORIENTED_EDGE ( 'NONE', *, *, #9040, .F. ) ;
#7950 = CARTESIAN_POINT ( 'NONE',  ( -4.340256562281096464, -97.38225965448614829, -6.691037544056555042 ) ) ;
#7951 = CARTESIAN_POINT ( 'NONE',  ( -25.00000000000000355, 120.0000000000000284, 0.5000000000000000000 ) ) ;
#7952 = DIRECTION ( 'NONE',  ( 0.000000000000000000, 0.000000000000000000, 1.000000000000000000 ) ) ;
#7954 = EDGE_LOOP ( 'NONE', ( #9221, #7771, #10633, #5383 ) ) ;
#7953 = VECTOR ( 'NONE', #12310, 1000.000000000000000 ) ;
#7955 = DIRECTION ( 'NONE',  ( 1.000000000000000000, 0.000000000000000000, 0.000000000000000000 ) ) ;
#7956 = VERTEX_POINT ( 'NONE', #7077 ) ;
#7957 = CARTESIAN_POINT ( 'NONE',  ( 1.912509855227740641, -139.1821000271621926, 2.327450852377690005 ) ) ;
#7958 = ADVANCED_FACE ( 'NONE', ( #12486 ), #12563, .T. ) ;
#7959 = CARTESIAN_POINT ( 'NONE',  ( 4.471182088707192470, 90.98125128669738615, -2.240943909473569473 ) ) ;
#7960 = CARTESIAN_POINT ( 'NONE',  ( -35.06230589874905235, 106.5835921350012825, 7.500000000000000000 ) ) ;
#7961 = VECTOR ( 'NONE', #7800, 999.9999999999998863 ) ;
#7962 = DIRECTION ( 'NONE',  ( 1.000000000000000000, 0.000000000000000000, 0.000000000000000000 ) ) ;
#7963 = DIRECTION ( 'NONE',  ( -1.000000000000000000, 0.000000000000000000, 0.000000000000000000 ) ) ;
#7964 = CARTESIAN_POINT ( 'NONE',  ( -40.81228451836347659, 100.6358150620708614, -0.6381026355483951917 ) ) ;
#7965 = DIRECTION ( 'NONE',  ( -2.797435172181481150E-17, 1.000000000000000000, -1.765856845898762549E-18 ) ) ;
#7966 = DIRECTION ( 'NONE',  ( -1.000000000000000000, 0.000000000000000000, 0.000000000000000000 ) ) ;
#7967 = CARTESIAN_POINT ( 'NONE',  ( -8.385254915620294014, 15.32944684068712782, 16.77050983124058092 ) ) ;
#7968 = CIRCLE ( 'NONE', #9536, 5.000000000000000000 ) ;
#7969 = VERTEX_POINT ( 'NONE', #5044 ) ;
#7970 = CARTESIAN_POINT ( 'NONE',  ( 2.771542151761392070, 90.01585036846415733, 4.174539845741942479 ) ) ;
#7971 = ORIENTED_EDGE ( 'NONE', *, *, #8397, .T. ) ;
#7972 = AXIS2_PLACEMENT_3D ( 'NONE', #9623, #13739, #10602 ) ;
#7973 = CARTESIAN_POINT ( 'NONE',  ( 1.111721538977011203, -76.35064935050891677, 4.681383094373183340 ) ) ;
#7974 = VECTOR ( 'NONE', #11448, 1000.000000000000000 ) ;
#7975 = ORIENTED_EDGE ( 'NONE', *, *, #11073, .F. ) ;
#7976 = DIRECTION ( 'NONE',  ( -1.000000000000000000, 0.000000000000000000, 0.000000000000000000 ) ) ;
#7977 = EDGE_CURVE ( 'NONE', #5594, #11832, #13712, .T. ) ;
#7978 = CONTEXT_DEPENDENT_SHAPE_REPRESENTATION ( #5757, #2376 ) ;
#7979 = ADVANCED_FACE ( 'NONE', ( #11826 ), #3274, .F. ) ;
#7980 = VECTOR ( 'NONE', #5360, 1000.000000000000000 ) ;
#7981 = CARTESIAN_POINT ( 'NONE',  ( 10.43546891138484511, -95.36363636363113017, 7.899666394170035133 ) ) ;
#7982 = CARTESIAN_POINT ( 'NONE',  ( 12.99579180576516002, 7.534841976936129448, 25.99158361153033070 ) ) ;
#7983 = CARTESIAN_POINT ( 'NONE',  ( -40.24692185806993194, 100.8304034607652255, 1.836112450589438838 ) ) ;
#7984 = AXIS2_PLACEMENT_3D ( 'NONE', #11984, #6656, #1322 ) ;
#7985 = CARTESIAN_POINT ( 'NONE',  ( -2.517691654963332357E-15, 90.00000000000000000, -1.589271161308885878E-16 ) ) ;
#7986 = PRODUCT_DEFINITION_CONTEXT ( 'detailed design', #8892, 'design' ) ;
#7987 = DIRECTION ( 'NONE',  ( -0.8000000000000008216, 0.5999999999999988676, 0.000000000000000000 ) ) ;
#7988 = VERTEX_POINT ( 'NONE', #5373 ) ;
#7989 = VERTEX_POINT ( 'NONE', #3527 ) ;
#7990 = EDGE_CURVE ( 'NONE', #13685, #3535, #3826, .T. ) ;
#7991 = ORIENTED_EDGE ( 'NONE', *, *, #8677, .F. ) ;
#7992 = ORIENTED_EDGE ( 'NONE', *, *, #4024, .F. ) ;
#7993 = CARTESIAN_POINT ( 'NONE',  ( -8.385254915620297567, -34.41905512736551032, -1.990698649637279025E-15 ) ) ;
#7994 = MANIFOLD_SOLID_BREP ( 'Mirror3', #5348 ) ;
#7995 = AXIS2_PLACEMENT_3D ( 'NONE', #8671, #12838, #6435 ) ;
#7996 = CARTESIAN_POINT ( 'NONE',  ( -35.00000000000000000, -4.286263797015736496E-15, -8.499999999999998224 ) ) ;
#7997 = EDGE_CURVE ( 'NONE', #2860, #7931, #8466, .T. ) ;
#7998 = CARTESIAN_POINT ( 'NONE',  ( 0.000000000000000000, 40.00000000000000000, 0.000000000000000000 ) ) ;
#7999 = EDGE_CURVE ( 'NONE', #7762, #3806, #10759, .T. ) ;
#8000 = CARTESIAN_POINT ( 'NONE',  ( -39.99999999999999289, 120.0000000000000142, -0.5000000000000000000 ) ) ;
#8001 = CARTESIAN_POINT ( 'NONE',  ( 0.9785323935166234666, -82.17131360862762790, -9.727322450732026837 ) ) ;
#8002 = CARTESIAN_POINT ( 'NONE',  ( 15.29705854078138216, 57.37192529142944863, 30.59411708156277854 ) ) ;
#8003 = ORIENTED_EDGE ( 'NONE', *, *, #2420, .T. ) ;
#8004 = ORIENTED_EDGE ( 'NONE', *, *, #1457, .T. ) ;
#8005 = PRODUCT_DEFINITION_SHAPE ( 'NONE', 'NONE',  #2214 ) ;
#8006 = EDGE_LOOP ( 'NONE', ( #1646, #11501, #8160, #2439 ) ) ;
#8007 = EDGE_CURVE ( 'NONE', #2559, #5941, #5391, .T. ) ;
#8008 = LINE ( 'NONE', #11232, #106 ) ;
#8009 = CARTESIAN_POINT ( 'NONE',  ( 2.142312913383998207, -80.12121212121218150, 9.955895698471858069 ) ) ;
#8010 =( BOUNDED_SURFACE ( )  B_SPLINE_SURFACE ( 3, 3, ( 
 ( #4159, #6473, #5480, #9765 ),
 ( #10740, #11932, #6543, #2323 ),
 ( #10869, #4566, #11798, #9832 ),
 ( #311, #5696, #1417, #9980 ) ),
 .UNSPECIFIED., .F., .F., .T. ) 
 B_SPLINE_SURFACE_WITH_KNOTS ( ( 4, 4 ),
 ( 4, 4 ),
 ( 0.000000000000000000, 1.000000000000000000 ),
 ( 0.000000000000000000, 1.000000000000000000 ),
 .UNSPECIFIED. ) 
 GEOMETRIC_REPRESENTATION_ITEM ( )  RATIONAL_B_SPLINE_SURFACE ( (
 ( 1.000000000000000000, 0.3333333333333334259, 0.3333333333333334259, 1.000000000000000000),
 ( 1.000000000000000000, 0.3333333333333334259, 0.3333333333333334259, 1.000000000000000000),
 ( 1.000000000000000000, 0.3333333333333334259, 0.3333333333333334259, 1.000000000000000000),
 ( 1.000000000000000000, 0.3333333333333334259, 0.3333333333333334259, 1.000000000000000000) ) ) 
 REPRESENTATION_ITEM ( '' )  SURFACE ( )  );
#8011 = ORIENTED_EDGE ( 'NONE', *, *, #9381, .T. ) ;
#8012 = CARTESIAN_POINT ( 'NONE',  ( 1.964926810246274247, -77.94210575524361673, 9.914063055205920350 ) ) ;
#8013 = LINE ( 'NONE', #2680, #4818 ) ;
#8014 = CARTESIAN_POINT ( 'NONE',  ( 5.925229457222553897, -117.0909090909068482, 2.047657493157430952 ) ) ;
#8015 = DIRECTION ( 'NONE',  ( -0.000000000000000000, -0.000000000000000000, -1.000000000000000000 ) ) ;
#8016 = CARTESIAN_POINT ( 'NONE',  ( -6.764234067550082941, -111.2727272727269821, 0.6609924544552703285 ) ) ;
#8017 = EDGE_CURVE ( 'NONE', #3902, #4278, #4477, .T. ) ;
#8018 = FACE_OUTER_BOUND ( 'NONE', #9596, .T. ) ;
#8019 = CARTESIAN_POINT ( 'NONE',  ( 15.18222645069203303, -16.04698886238941924, -4.000000000000000000 ) ) ;
#8020 = DIRECTION ( 'NONE',  ( -1.000000000000000000, 0.000000000000000000, 0.000000000000000000 ) ) ;
#8021 = VERTEX_POINT ( 'NONE', #9021 ) ;
#8022 = VERTEX_POINT ( 'NONE', #13408 ) ;
#8023 = ORIENTED_EDGE ( 'NONE', *, *, #8185, .F. ) ;
#8024 = CARTESIAN_POINT ( 'NONE',  ( -3.661863250968810046, -131.0369695719847982, 1.478767330369552768 ) ) ;
#8025 = DIRECTION ( 'NONE',  ( -5.551115123125776539E-17, 1.000000000000000000, 3.944304526105059027E-31 ) ) ;
#8026 = DIRECTION ( 'NONE',  ( 1.000000000000000000, 1.224646799147353207E-16, 0.000000000000000000 ) ) ;
#8027 = FACE_OUTER_BOUND ( 'NONE', #25, .T. ) ;
#8028 = DIRECTION ( 'NONE',  ( -0.000000000000000000, -0.000000000000000000, -1.000000000000000000 ) ) ;
#8029 = ORIENTED_EDGE ( 'NONE', *, *, #13514, .F. ) ;
#8030 = DIRECTION ( 'NONE',  ( 0.000000000000000000, -1.000000000000000000, 0.000000000000000000 ) ) ;
#8031 = VERTEX_POINT ( 'NONE', #12458 ) ;
#8032 = DIRECTION ( 'NONE',  ( -1.000000000000000000, 0.000000000000000000, 0.000000000000000000 ) ) ;
#8033 = CARTESIAN_POINT ( 'NONE',  ( -31.81818181818181657, 133.3608531424536920, 2.500000000000000000 ) ) ;
#8034 = CARTESIAN_POINT ( 'NONE',  ( -34.24999999999972999, -135.0000000000000000, -4.194415287079653581E-15 ) ) ;
#8035 = PLANE ( 'NONE',  #9400 ) ;
#8036 = CARTESIAN_POINT ( 'NONE',  ( 1.947606478028208261E-13, -70.00000000000000000, 2.411204079342396664E-14 ) ) ;
#8037 = LINE ( 'NONE', #2709, #10323 ) ;
#8038 = FACE_OUTER_BOUND ( 'NONE', #8581, .T. ) ;
#8039 = AXIS2_PLACEMENT_3D ( 'NONE', #1967, #3148, #10652 ) ;
#8040 = VERTEX_POINT ( 'NONE', #3824 ) ;
#8041 = CARTESIAN_POINT ( 'NONE',  ( 3.523137085080620956, 90.23509738553477177, 3.551515709300293366 ) ) ;
#8042 = CARTESIAN_POINT ( 'NONE',  ( 18.84535726572642034, -167.3636363553120532, 7.741214183180429309 ) ) ;
#8043 = ORIENTED_EDGE ( 'NONE', *, *, #12876, .F. ) ;
#8044 = ORIENTED_EDGE ( 'NONE', *, *, #2592, .F. ) ;
#8045 = CARTESIAN_POINT ( 'NONE',  ( -25.00000000000000355, 120.0000000000000142, 2.499999999999999556 ) ) ;
#8046 = CARTESIAN_POINT ( 'NONE',  ( 17.38503225228318883, -6.421675190136373779, -2.500000000000002665 ) ) ;
#8047 = CARTESIAN_POINT ( 'NONE',  ( -3.784192700541033183, -169.0000000000003126, -1.982393907671172961 ) ) ;
#8048 = CARTESIAN_POINT ( 'NONE',  ( -40.49366238756161351, 100.7360090884195500, 1.526167340029800146 ) ) ;
#8049 = CARTESIAN_POINT ( 'NONE',  ( -35.00000000000000000, 25.00000000000000000, 7.500000000000000000 ) ) ;
#8050 = AXIS2_PLACEMENT_3D ( 'NONE', #4554, #5402, #10925 ) ;
#8051 = CARTESIAN_POINT ( 'NONE',  ( 6.266477192377021943, -76.69310173738496417, 7.966230643697302938 ) ) ;
#8052 = ORIENTED_EDGE ( 'NONE', *, *, #7896, .F. ) ;
#8053 = ORIENTED_EDGE ( 'NONE', *, *, #4702, .F. ) ;
#8054 = CARTESIAN_POINT ( 'NONE',  ( 16.53267785980283477, 10.29504797295195573, 2.500000000000001776 ) ) ;
#8055 = PRODUCT_DEFINITION ( 'UNKNOWN', '', #4155, #12338 ) ;
#8056 = CIRCLE ( 'NONE', #10733, 80.00000000000001421 ) ;
#8057 = ORIENTED_EDGE ( 'NONE', *, *, #4916, .F. ) ;
#8058 = CARTESIAN_POINT ( 'NONE',  ( -10.69346802281034670, -25.79937747632526879, -1.218456123918935934E-15 ) ) ;
#8059 = CIRCLE ( 'NONE', #13702, 9.000000000008999024 ) ;
#8060 = CARTESIAN_POINT ( 'NONE',  ( -8.385254915620301119, 78.67828027274755698, 16.77050983124059158 ) ) ;
#8061 = DIRECTION ( 'NONE',  ( -0.000000000000000000, -0.000000000000000000, -1.000000000000000000 ) ) ;
#8062 =( BOUNDED_SURFACE ( )  B_SPLINE_SURFACE ( 3, 3, ( 
 ( #4320, #474, #8599, #13251 ),
 ( #1358, #12903, #2407, #5638 ),
 ( #3457, #3523, #12168, #6689 ),
 ( #12753, #11690, #7736, #2084 ) ),
 .UNSPECIFIED., .F., .F., .T. ) 
 B_SPLINE_SURFACE_WITH_KNOTS ( ( 4, 4 ),
 ( 4, 4 ),
 ( 0.000000000000000000, 1.000000000000000000 ),
 ( 0.000000000000000000, 1.000000000000000000 ),
 .UNSPECIFIED. ) 
 GEOMETRIC_REPRESENTATION_ITEM ( )  RATIONAL_B_SPLINE_SURFACE ( (
 ( 1.000000000000000000, 0.3333333333333334259, 0.3333333333333334259, 1.000000000000000000),
 ( 1.000000000000000000, 0.3333333333333334259, 0.3333333333333334259, 1.000000000000000000),
 ( 1.000000000000000000, 0.3333333333333334259, 0.3333333333333334259, 1.000000000000000000),
 ( 1.000000000000000000, 0.3333333333333334259, 0.3333333333333334259, 1.000000000000000000) ) ) 
 REPRESENTATION_ITEM ( '' )  SURFACE ( )  );
#8063 = FACE_OUTER_BOUND ( 'NONE', #6014, .T. ) ;
#8064 = CARTESIAN_POINT ( 'NONE',  ( -1.147385087825261607, -80.61700017096171678, -9.985132701286346446 ) ) ;
#8065 = CARTESIAN_POINT ( 'NONE',  ( -15.29705854078138394, 17.78624592198638155, -30.59411708156277854 ) ) ;
#8066 = EDGE_LOOP ( 'NONE', ( #3211, #9039, #13373, #10597 ) ) ;
#8067 = EDGE_CURVE ( 'NONE', #12537, #11430, #10974, .T. ) ;
#8068 = VECTOR ( 'NONE', #1534, 1000.000000000000000 ) ;
#8069 = EDGE_LOOP ( 'NONE', ( #4166, #9876, #9421, #12139 ) ) ;
#8070 = EDGE_CURVE ( 'NONE', #9516, #1833, #11214, .T. ) ;
#8071 = EDGE_CURVE ( 'NONE', #1714, #11917, #5789, .T. ) ;
#8072 = CARTESIAN_POINT ( 'NONE',  ( -8.256647985966802494, -92.46527916421074167, -2.505673630511644934 ) ) ;
#8073 = CIRCLE ( 'NONE', #12570, 27.49999999999999289 ) ;
#8074 = CARTESIAN_POINT ( 'NONE',  ( -10.69346802281035025, -6.949821576306441706, 21.38693604562069339 ) ) ;
#8075 = EDGE_CURVE ( 'NONE', #6545, #7000, #616, .T. ) ;
#8076 = EDGE_CURVE ( 'NONE', #7525, #4575, #6727, .T. ) ;
#8077 = ORIENTED_EDGE ( 'NONE', *, *, #5940, .T. ) ;
#8078 = DIRECTION ( 'NONE',  ( -0.000000000000000000, -0.000000000000000000, -1.000000000000000000 ) ) ;
#8079 = CARTESIAN_POINT ( 'NONE',  ( 4.858750903448073366, -78.09090909090949140, 8.996753037508748108 ) ) ;
#8080 = ORIENTED_EDGE ( 'NONE', *, *, #9857, .F. ) ;
#8081 = CARTESIAN_POINT ( 'NONE',  ( 4.471144793536856454, 90.98178511618806397, 2.240986362385854580 ) ) ;
#8082 =( NAMED_UNIT ( * ) PLANE_ANGLE_UNIT ( ) SI_UNIT ( $, .RADIAN. ) );
#8083 = VECTOR ( 'NONE', #2779, 1000.000000000000000 ) ;
#8084 = DIRECTION ( 'NONE',  ( 0.9960067511297464593, -0.08927794634716622324, 3.401418580343279473E-17 ) ) ;
#8085 = CARTESIAN_POINT ( 'NONE',  ( -15.29705854078138749, 10.24803554138234496, -1.809656371776380929E-17 ) ) ;
#8086 = CARTESIAN_POINT ( 'NONE',  ( -5.494716852924834249, -106.9090909090907502, 4.862358660864143367 ) ) ;
#8087 = CIRCLE ( 'NONE', #10315, 4.999999999999998224 ) ;
#8088 = FACE_OUTER_BOUND ( 'NONE', #1865, .T. ) ;
#8089 = AXIS2_PLACEMENT_3D ( 'NONE', #7286, #9190, #9333 ) ;
#8090 = FACE_OUTER_BOUND ( 'NONE', #8006, .T. ) ;
#8091 = ORIENTED_EDGE ( 'NONE', *, *, #8570, .F. ) ;
#8092 = EDGE_LOOP ( 'NONE', ( #7501, #9555, #2472, #11945 ) ) ;
#8093 = DIRECTION ( 'NONE',  ( -0.000000000000000000, -0.000000000000000000, -1.000000000000000000 ) ) ;
#8094 = VERTEX_POINT ( 'NONE', #3679 ) ;
#8095 = CARTESIAN_POINT ( 'NONE',  ( 6.191228697746712584, -110.8526145195744306, -1.341853914380320978 ) ) ;
#8096 = CARTESIAN_POINT ( 'NONE',  ( -35.00000000000000000, -4.286263797015736496E-15, 4.000000000000000000 ) ) ;
#8097 = ADVANCED_FACE ( 'NONE', ( #6071 ), #12525, .T. ) ;
#8098 = VECTOR ( 'NONE', #11148, 1000.000000000000000 ) ;
#8099 = VECTOR ( 'NONE', #8093, 1000.000000000000000 ) ;
#8100 = CARTESIAN_POINT ( 'NONE',  ( 0.000000000000000000, 71.01020514433645303, 0.5000000000000000000 ) ) ;
#8101 = CARTESIAN_POINT ( 'NONE',  ( -4.975586992323414874E-16, 17.78624592198638155, -3.140796412417860432E-17 ) ) ;
#8102 = ORIENTED_EDGE ( 'NONE', *, *, #11827, .F. ) ;
#8103 = CARTESIAN_POINT ( 'NONE',  ( -49.99999999999999289, 120.0000000000000284, 0.5000000000000000000 ) ) ;
#8104 = CARTESIAN_POINT ( 'NONE',  ( 2.989041064089018374, -128.2926750340500917, -3.053002924880402702 ) ) ;
#8105 = CARTESIAN_POINT ( 'NONE',  ( -36.36363636363635976, 142.2680885707561629, 0.5000000000000000000 ) ) ;
#8106 = DIRECTION ( 'NONE',  ( 1.000000000000000000, 0.000000000000000000, 0.000000000000000000 ) ) ;
#8107 = CARTESIAN_POINT ( 'NONE',  ( 28.79177319725820183, -26.24642857144861807, -4.000000000000000000 ) ) ;
#8108 = CARTESIAN_POINT ( 'NONE',  ( -10.00000000000000000, 99.99999999999994316, 2.500000000000000000 ) ) ;
#8109 = CARTESIAN_POINT ( 'NONE',  ( -15.29705854078139105, 47.94714734142005597, -8.466779837416320124E-17 ) ) ;
#8110 = AXIS2_PLACEMENT_3D ( 'NONE', #307, #9827, #5619 ) ;
#8111 = ORIENTED_EDGE ( 'NONE', *, *, #2997, .F. ) ;
#8112 = DIRECTION ( 'NONE',  ( -1.000000000000000000, 0.000000000000000000, 0.000000000000000000 ) ) ;
#8113 = VERTEX_POINT ( 'NONE', #1782 ) ;
#8114 = CARTESIAN_POINT ( 'NONE',  ( 11.95302590260997455, -161.0909090909845816, 5.173310689862941736 ) ) ;
#8115 = ADVANCED_FACE ( 'NONE', ( #749 ), #3591, .T. ) ;
#8116 = ORIENTED_EDGE ( 'NONE', *, *, #6269, .F. ) ;
#8117 = EDGE_LOOP ( 'NONE', ( #3377, #854, #6637, #8111 ) ) ;
#8118 = DIRECTION ( 'NONE',  ( 1.000000000000000000, -5.551115123125785069E-15, 0.000000000000000000 ) ) ;
#8119 = DIRECTION ( 'NONE',  ( -6.158143864569485777E-17, -2.736152283717910599E-16, 1.000000000000000000 ) ) ;
#8120 = VECTOR ( 'NONE', #951, 1000.000000000000000 ) ;
#8121 = CARTESIAN_POINT ( 'NONE',  ( -6.139211203638544667, -76.35064935069904379, -12.15884065890355181 ) ) ;
#8122 = DIRECTION ( 'NONE',  ( 0.000000000000000000, 0.000000000000000000, 1.000000000000000000 ) ) ;
#8123 = DIRECTION ( 'NONE',  ( -0.000000000000000000, -0.000000000000000000, -1.000000000000000000 ) ) ;
#8124 = DIRECTION ( 'NONE',  ( 0.8907235428302453517, -0.4545454545454570838, 0.000000000000000000 ) ) ;
#8125 = ORIENTED_EDGE ( 'NONE', *, *, #10710, .F. ) ;
#8126 = DIRECTION ( 'NONE',  ( 1.000000000000000000, 0.000000000000000000, 0.000000000000000000 ) ) ;
#8127 = AXIS2_PLACEMENT_3D ( 'NONE', #10771, #5443, #9731 ) ;
#8128 = ORIENTED_EDGE ( 'NONE', *, *, #12391, .T. ) ;
#8129 = CIRCLE ( 'NONE', #5208, 9.000000000009000800 ) ;
#8130 = EDGE_CURVE ( 'NONE', #12373, #6030, #2475, .T. ) ;
#8131 = CARTESIAN_POINT ( 'NONE',  ( 8.385254915620288685, 78.67828027274755698, 16.77050983124059158 ) ) ;
#8132 = CARTESIAN_POINT ( 'NONE',  ( -12.99579180576516713, -1.889935973073298525, -3.189601575276258806E-15 ) ) ;
#8133 = DIRECTION ( 'NONE',  ( -0.000000000000000000, -0.000000000000000000, -1.000000000000000000 ) ) ;
#8134 = CARTESIAN_POINT ( 'NONE',  ( -5.810149393362634918, -114.7767544601693430, 0.9592521923076761103 ) ) ;
#8135 = CARTESIAN_POINT ( 'NONE',  ( -8.385254915620290461, -31.79444290936001494, -16.77050983124059158 ) ) ;
#8136 = ORIENTED_EDGE ( 'NONE', *, *, #2761, .T. ) ;
#8137 = AXIS2_PLACEMENT_3D ( 'NONE', #5329, #8552, #13543 ) ;
#8138 = ORIENTED_EDGE ( 'NONE', *, *, #6870, .F. ) ;
#8139 = ORIENTED_EDGE ( 'NONE', *, *, #12822, .F. ) ;
#8140 = DIRECTION ( 'NONE',  ( -1.000000000000000000, 0.000000000000000000, 0.000000000000000000 ) ) ;
#8141 = CARTESIAN_POINT ( 'NONE',  ( -12.99553232110414847, -26.62435705548576692, 25.99106464220827917 ) ) ;
#8142 = VECTOR ( 'NONE', #3649, 1000.000000000000000 ) ;
#8143 = DIRECTION ( 'NONE',  ( -2.797435172181481150E-17, 1.000000000000000000, -1.765856845898762549E-18 ) ) ;
#8144 = ORIENTED_EDGE ( 'NONE', *, *, #11056, .T. ) ;
#8145 = LINE ( 'NONE', #6811, #10803 ) ;
#8146 =( BOUNDED_SURFACE ( )  B_SPLINE_SURFACE ( 3, 3, ( 
 ( #356, #3774, #4614, #7757 ),
 ( #10018, #5892, #13428, #12343 ),
 ( #7919, #12199, #13119, #2517 ),
 ( #2733, #2588, #6866, #13203 ) ),
 .UNSPECIFIED., .F., .F., .T. ) 
 B_SPLINE_SURFACE_WITH_KNOTS ( ( 4, 4 ),
 ( 4, 4 ),
 ( 0.000000000000000000, 1.000000000000000000 ),
 ( 0.000000000000000000, 1.000000000000000000 ),
 .UNSPECIFIED. ) 
 GEOMETRIC_REPRESENTATION_ITEM ( )  RATIONAL_B_SPLINE_SURFACE ( (
 ( 1.000000000000000000, 0.3333333333333334259, 0.3333333333333334259, 1.000000000000000000),
 ( 1.000000000000000000, 0.3333333333333334259, 0.3333333333333334259, 1.000000000000000000),
 ( 1.000000000000000000, 0.3333333333333334259, 0.3333333333333334259, 1.000000000000000000),
 ( 1.000000000000000000, 0.3333333333333334259, 0.3333333333333334259, 1.000000000000000000) ) ) 
 REPRESENTATION_ITEM ( '' )  SURFACE ( )  );
#8147 = ADVANCED_FACE ( 'NONE', ( #6904 ), #12578, .T. ) ;
#8148 = FACE_OUTER_BOUND ( 'NONE', #4956, .T. ) ;
#8149 = DIRECTION ( 'NONE',  ( -1.000000000000000000, -1.224646799147353207E-16, 0.000000000000000000 ) ) ;
#8150 = CARTESIAN_POINT ( 'NONE',  ( -5.925229457222161322, -117.0909090909115235, -2.047657493157731157 ) ) ;
#8151 = FACE_OUTER_BOUND ( 'NONE', #4115, .T. ) ;
#8152 = DIRECTION ( 'NONE',  ( -1.000000000000000000, 0.000000000000000000, 0.000000000000000000 ) ) ;
#8153 = EDGE_CURVE ( 'NONE', #12537, #5686, #5872, .T. ) ;
#8154 = DIRECTION ( 'NONE',  ( -0.000000000000000000, -0.000000000000000000, -1.000000000000000000 ) ) ;
#8155 = EDGE_CURVE ( 'NONE', #357, #3902, #8037, .T. ) ;
#8156 = ORIENTED_EDGE ( 'NONE', *, *, #3023, .T. ) ;
#8157 = ORIENTED_EDGE ( 'NONE', *, *, #12356, .T. ) ;
#8158 = ORIENTED_EDGE ( 'NONE', *, *, #7990, .T. ) ;
#8159 = DIRECTION ( 'NONE',  ( 1.000000000000000000, 0.000000000000000000, 0.000000000000000000 ) ) ;
#8160 = ORIENTED_EDGE ( 'NONE', *, *, #984, .F. ) ;
#8161 = AXIS2_PLACEMENT_3D ( 'NONE', #3079, #5251, #9539 ) ;
#8162 = CARTESIAN_POINT ( 'NONE',  ( -2.946076804534930815, -128.2487050844958674, 3.060050242327970071 ) ) ;
#8163 = DIRECTION ( 'NONE',  ( 0.8035603370713739757, 0.5952233065713573579, 0.000000000000000000 ) ) ;
#8164 = FACE_OUTER_BOUND ( 'NONE', #8066, .T. ) ;
#8165 = EDGE_LOOP ( 'NONE', ( #246, #10164, #10123, #13861 ) ) ;
#8166 = DIRECTION ( 'NONE',  ( 0.000000000000000000, 1.000000000000000000, 2.775557561562888984E-15 ) ) ;
#8167 = CARTESIAN_POINT ( 'NONE',  ( -0.4690429436946310093, -122.4721769046603868, -4.906597864725500635 ) ) ;
#8168 = DIRECTION ( 'NONE',  ( -0.000000000000000000, -0.000000000000000000, 1.000000000000000000 ) ) ;
#8169 = CARTESIAN_POINT ( 'NONE',  ( 15.29705854078138927, 90.00000000000000000, 1.714422261702872766E-15 ) ) ;
#8170 = CARTESIAN_POINT ( 'NONE',  ( 4.355466475183198247E-16, -15.56949922734665570, 2.749350679782564022E-17 ) ) ;
#8171 = FACE_OUTER_BOUND ( 'NONE', #1459, .T. ) ;
#8172 = DIRECTION ( 'NONE',  ( 0.000000000000000000, 0.000000000000000000, 1.000000000000000000 ) ) ;
#8173 = CYLINDRICAL_SURFACE ( 'NONE', #911, 2.000000000000000000 ) ;
#8174 = ADVANCED_FACE ( 'NONE', ( #2842 ), #8173, .T. ) ;
#8175 = CARTESIAN_POINT ( 'NONE',  ( 15.29705854078138749, 64.91013567203349055, 30.59411708156278564 ) ) ;
#8176 = EDGE_CURVE ( 'NONE', #10854, #10350, #6008, .T. ) ;
#8177 = EDGE_LOOP ( 'NONE', ( #3671, #72, #7798, #2294, #5036 ) ) ;
#8178 = CARTESIAN_POINT ( 'NONE',  ( -10.91573825925852859, -140.5584415584503404, -8.453432789889644638 ) ) ;
#8179 = AXIS2_PLACEMENT_3D ( 'NONE', #180, #5703, #3381 ) ;
#8180 = VERTEX_POINT ( 'NONE', #13544 ) ;
#8181 = TOROIDAL_SURFACE ( 'NONE', #13362, 16.99999999999998934, 2.000000000000000000 ) ;
#8182 = VERTEX_POINT ( 'NONE', #3894 ) ;
#8183 = CARTESIAN_POINT ( 'NONE',  ( -4.471144793536862672, 90.98178511618806397, -2.240986362385854580 ) ) ;
#8184 = FACE_OUTER_BOUND ( 'NONE', #4450, .T. ) ;
#8185 = EDGE_CURVE ( 'NONE', #11917, #10214, #11442, .T. ) ;
#8186 = CARTESIAN_POINT ( 'NONE',  ( -11.72298137502704840, -61.00000000000002842, -2.970135970080977739 ) ) ;
#8187 = CARTESIAN_POINT ( 'NONE',  ( 8.385254915620292238, 5.904668890677672088, 2.053795118489800004E-15 ) ) ;
#8188 = LINE ( 'NONE', #11342, #11785 ) ;
#8189 = CIRCLE ( 'NONE', #2126, 8.385254915620294014 ) ;
#8190 = EDGE_CURVE ( 'NONE', #9553, #12643, #5171, .T. ) ;
#8191 = FACE_OUTER_BOUND ( 'NONE', #7585, .T. ) ;
#8192 = DIRECTION ( 'NONE',  ( -2.797435172181481150E-17, 1.000000000000000000, -1.765856845898762549E-18 ) ) ;
#8193 = AXIS2_PLACEMENT_3D ( 'NONE', #1409, #10931, #382 ) ;
#8194 = TOROIDAL_SURFACE ( 'NONE', #13609, 16.99999999999998934, 2.000000000000000000 ) ;
#8195 = ORIENTED_EDGE ( 'NONE', *, *, #4210, .T. ) ;
#8196 = ORIENTED_EDGE ( 'NONE', *, *, #3710, .F. ) ;
#8197 = DIRECTION ( 'NONE',  ( 5.337610695313252124E-17, -1.000000000000000000, 0.000000000000000000 ) ) ;
#8198 = CIRCLE ( 'NONE', #2362, 1.999999999999998224 ) ;
#8199 = PRODUCT_DEFINITION_FORMATION_WITH_SPECIFIED_SOURCE ( 'ANY', '', #3279, .NOT_KNOWN. ) ;
#8200 = ORIENTED_EDGE ( 'NONE', *, *, #7222, .T. ) ;
#8201 = CARTESIAN_POINT ( 'NONE',  ( -10.00000000000000711, 99.99999999999994316, 2.500000000000000000 ) ) ;
#8202 = AXIS2_PLACEMENT_3D ( 'NONE', #946, #6336, #12523 ) ;
#8203 = CARTESIAN_POINT ( 'NONE',  ( -12.99553232110414314, 29.92431064457076673, -3.246435148940206039E-15 ) ) ;
#8204 = FACE_OUTER_BOUND ( 'NONE', #1528, .T. ) ;
#8205 = DIRECTION ( 'NONE',  ( -0.4545454545454531425, 0.8907235428302472391, 0.000000000000000000 ) ) ;
#8206 = CARTESIAN_POINT ( 'NONE',  ( 2.607178694270818831, -83.43640819696341282, -9.281062047519146319 ) ) ;
#8207 = CARTESIAN_POINT ( 'NONE',  ( 1.958204620527036102E-15, -69.99999999999998579, 1.236099792129133461E-16 ) ) ;
#8208 = ORIENTED_EDGE ( 'NONE', *, *, #9849, .T. ) ;
#8209 = EDGE_LOOP ( 'NONE', ( #9819, #933, #3644, #7089 ) ) ;
#8210 = DIRECTION ( 'NONE',  ( 1.000000000000000000, 0.000000000000000000, 0.000000000000000000 ) ) ;
#8211 = AXIS2_PLACEMENT_3D ( 'NONE', #5098, #13759, #9454 ) ;
#8212 = CARTESIAN_POINT ( 'NONE',  ( 39.06230589874904524, 109.5835921350012683, -2.499999999999998668 ) ) ;
#8213 = EDGE_LOOP ( 'NONE', ( #6827, #91 ) ) ;
#8214 = CARTESIAN_POINT ( 'NONE',  ( 39.06230589874905235, 109.5835921350012683, -2.499999999999999556 ) ) ;
#8215 = CARTESIAN_POINT ( 'NONE',  ( -31.93204061526058624, -132.0000000000000000, 0.000000000000000000 ) ) ;
#8216 = CARTESIAN_POINT ( 'NONE',  ( -1.026257020618903670, -73.45454545136195179, -21.46608457335733178 ) ) ;
#8217 = FACE_BOUND ( 'NONE', #9335, .T. ) ;
#8218 = CARTESIAN_POINT ( 'NONE',  ( -0.03701750592458041833, -157.3626971396553529, -1.516132001818238706 ) ) ;
#8219 = CARTESIAN_POINT ( 'NONE',  ( 10.00000000000000000, 90.00000000000000000, 2.500000000000000000 ) ) ;
#8220 = ORIENTED_EDGE ( 'NONE', *, *, #2247, .F. ) ;
#8221 = AXIS2_PLACEMENT_3D ( 'NONE', #4742, #9020, #4813 ) ;
#8222 = ORIENTED_EDGE ( 'NONE', *, *, #2516, .F. ) ;
#8223 = EDGE_CURVE ( 'NONE', #6698, #8382, #8735, .T. ) ;
#8224 = CARTESIAN_POINT ( 'NONE',  ( 3.364289002660265204, -118.5204725339004597, 4.219879093570879647 ) ) ;
#8225 = ADVANCED_FACE ( 'NONE', ( #5346 ), #1013, .T. ) ;
#8226 = CYLINDRICAL_SURFACE ( 'NONE', #263, 15.29705854078139105 ) ;
#8227 = CARTESIAN_POINT ( 'NONE',  ( -32.95454545454546746, 135.5876619995293311, -2.499999999999998668 ) ) ;
#8228 = CARTESIAN_POINT ( 'NONE',  ( -8.385254915620292238, 22.12961257269105531, -3.907772785857374249E-17 ) ) ;
#8229 = VERTEX_POINT ( 'NONE', #7316 ) ;
#8230 = DIRECTION ( 'NONE',  ( -1.000000000000000000, 0.000000000000000000, 0.000000000000000000 ) ) ;
#8231 = PLANE ( 'NONE',  #13294 ) ;
#8232 = CARTESIAN_POINT ( 'NONE',  ( -1.066429238991507766, -167.9999999999998863, 0.4719413927851786594 ) ) ;
#8233 = CARTESIAN_POINT ( 'NONE',  ( -8.385254915620292238, -22.36966495935058319, 3.950162600893091522E-17 ) ) ;
#8234 = CARTESIAN_POINT ( 'NONE',  ( -12.99553232110413425, 20.49953269456136695, -25.99106464220827917 ) ) ;
#8235 = CYLINDRICAL_SURFACE ( 'NONE', #8202, 9.000000000008999024 ) ;
#8236 = CARTESIAN_POINT ( 'NONE',  ( 15.29705854078139282, 90.00000000000000000, 1.714422261702873160E-15 ) ) ;
#8237 = CARTESIAN_POINT ( 'NONE',  ( -12.99553232110414314, 29.92431064457076673, -1.697177803646649065E-15 ) ) ;
#8238 = EDGE_CURVE ( 'NONE', #2048, #1705, #13501, .T. ) ;
#8239 = ORIENTED_EDGE ( 'NONE', *, *, #452, .T. ) ;
#8240 = DIRECTION ( 'NONE',  ( 0.000000000000000000, 0.000000000000000000, 1.000000000000000000 ) ) ;
#8241 = ORIENTED_EDGE ( 'NONE', *, *, #5748, .F. ) ;
#8242 = CARTESIAN_POINT ( 'NONE',  ( 12.05308885558885024, -134.6363636363533942, -5.101645771607613788 ) ) ;
#8243 = EDGE_CURVE ( 'NONE', #12375, #9005, #9435, .T. ) ;
#8244 = ORIENTED_EDGE ( 'NONE', *, *, #950, .T. ) ;
#8245 = EDGE_CURVE ( 'NONE', #2481, #12788, #1551, .T. ) ;
#8246 = ORIENTED_EDGE ( 'NONE', *, *, #8380, .F. ) ;
#8247 = CARTESIAN_POINT ( 'NONE',  ( -8.385254915620294014, 90.00000000000000000, -1.589271161308885878E-16 ) ) ;
#8248 = EDGE_CURVE ( 'NONE', #988, #5397, #6950, .T. ) ;
#8249 = CARTESIAN_POINT ( 'NONE',  ( 8.385254915620292238, 59.82872437272870769, 9.189312520034297072E-16 ) ) ;
#8250 = CARTESIAN_POINT ( 'NONE',  ( 15.49491024508755999, -22.63688244086936763, -2.616826951557488457 ) ) ;
#8251 = CARTESIAN_POINT ( 'NONE',  ( -8.385254915620292238, 34.17900274070598243, -2.138129980707100895E-15 ) ) ;
#8252 = AXIS2_PLACEMENT_3D ( 'NONE', #4621, #5456, #8902 ) ;
#8253 = CARTESIAN_POINT ( 'NONE',  ( 0.000000000000000000, 71.01020514433645303, 7.500000000000000000 ) ) ;
#8254 = CARTESIAN_POINT ( 'NONE',  ( -12.99553232110414314, 48.77386654458962312, -1.763749038303048460E-15 ) ) ;
#8255 = CARTESIAN_POINT ( 'NONE',  ( 15.29705854078138927, 90.00000000000000000, 1.714422261702872766E-15 ) ) ;
#8256 = DIRECTION ( 'NONE',  ( -2.797435172181481150E-17, 1.000000000000000000, -1.765856845898762549E-18 ) ) ;
#8257 = AXIS2_PLACEMENT_3D ( 'NONE', #6239, #1751, #7149 ) ;
#8258 = EDGE_LOOP ( 'NONE', ( #12814, #8582, #507, #3981, #5833, #1898 ) ) ;
#8259 = EDGE_CURVE ( 'NONE', #11738, #13355, #5378, .T. ) ;
#8260 = AXIS2_PLACEMENT_3D ( 'NONE', #9132, #654, #12428 ) ;
#8261 = CARTESIAN_POINT ( 'NONE',  ( -21.99999999999999289, -100.0000000000000000, 7.500000000000000000 ) ) ;
#8262 = ADVANCED_FACE ( 'NONE', ( #9432 ), #9564, .T. ) ;
#8263 = ORIENTED_EDGE ( 'NONE', *, *, #4727, .F. ) ;
#8264 = ORIENTED_EDGE ( 'NONE', *, *, #5886, .F. ) ;
#8265 = CARTESIAN_POINT ( 'NONE',  ( 8.385254915620292238, -22.36966495935058319, 1.068716529980328543E-15 ) ) ;
#8266 = CARTESIAN_POINT ( 'NONE',  ( -25.00000000000000355, 120.0000000000000142, 7.500000000000000000 ) ) ;
#8267 = VECTOR ( 'NONE', #8595, 1000.000000000000000 ) ;
#8268 = CARTESIAN_POINT ( 'NONE',  ( -10.69346802281034314, 30.74929022373127196, -21.38693604562069694 ) ) ;
#8269 = CARTESIAN_POINT ( 'NONE',  ( 8.385254915620294014, -3.520109059331755219, -16.77050983124058092 ) ) ;
#8270 = CARTESIAN_POINT ( 'NONE',  ( -0.005328072727578240381, -157.8884954289838447, 1.500081365927933508 ) ) ;
#8271 = CLOSED_SHELL ( 'NONE', ( #5778, #12085, #9872, #4872, #8332, #10856, #1725, #6176, #193, #2387, #8851, #9336, #5754, #192, #12236, #10790, #9598, #4120, #4978, #4630, #8642, #12103, #6681, #3125, #4531, #9028, #3170, #3410, #8573, #13846, #10440, #1379, #5415, #3595, #1210, #1312, #12311, #10706, #10900, #9026, #7437, #11050, #3530, #11687, #12379, #1394, #12569, #11347, #5500, #176, #12060, #2758, #3697, #7629, #12880, #4626, #7703, #4481, #631, #5835, #503, #1048, #5849, #11656, #12686, #4286, #7046, #11428, #5304, #2068, #6444, #1360, #7849, #5874, #3332, #2007, #4396, #10384, #12633, #12806, #13607, #11157, #4735, #1838, #3600, #3395, #9030, #6872, #21, #13340, #1303, #5020, #955, #10157, #8560, #10307, #5487, #4008, #10782, #2426, #13680, #8174, #7354, #12206, #4967, #10029, #7979, #935, #9393, #949, #10032, #500, #6111, #5324, #10877, #3778, #11486, #10724, #8097, #198, #10152, #8665, #10326, #3448, #8920, #13850, #8814, #7016, #8869, #4541, #6024, #5041, #10403, #7306, #10033, #8661, #11654, #4982, #7230, #9458, #13054, #13037, #2503, #7932, #2302, #9443, #5921, #3339, #3427, #2826, #9768, #3353, #2667, #1796, #6288, #8601, #5960, #3268, #1648, #7539, #112, #850, #13133, #1523, #7037, #9180, #5156, #12651, #1136, #8812, #13156 ) ) ;
#8272 = DIRECTION ( 'NONE',  ( 0.000000000000000000, 0.000000000000000000, 1.000000000000000000 ) ) ;
#8273 = VERTEX_POINT ( 'NONE', #10674 ) ;
#8274 = ORIENTED_EDGE ( 'NONE', *, *, #5316, .T. ) ;
#8275 = ORIENTED_EDGE ( 'NONE', *, *, #4210, .F. ) ;
#8276 = CIRCLE ( 'NONE', #4018, 2.000000000000000000 ) ;
#8277 = ORIENTED_EDGE ( 'NONE', *, *, #7116, .T. ) ;
#8278 = LINE ( 'NONE', #6185, #12194 ) ;
#8279 = AXIS2_PLACEMENT_3D ( 'NONE', #7035, #6829, #11314 ) ;
#8280 = ORIENTED_EDGE ( 'NONE', *, *, #776, .T. ) ;
#8281 = CARTESIAN_POINT ( 'NONE',  ( 6.150798755069183166, -74.45454545454636275, 8.129532795066678474 ) ) ;
#8282 = VERTEX_POINT ( 'NONE', #12874 ) ;
#8283 = CYLINDRICAL_SURFACE ( 'NONE', #11282, 9.000000000008999024 ) ;
#8284 = DIRECTION ( 'NONE',  ( 0.000000000000000000, 0.000000000000000000, 1.000000000000000000 ) ) ;
#8285 = DIRECTION ( 'NONE',  ( 1.000000000000000000, 0.000000000000000000, 0.000000000000000000 ) ) ;
#8286 = DIRECTION ( 'NONE',  ( -0.000000000000000000, 1.000000000000000000, -0.000000000000000000 ) ) ;
#8287 = CIRCLE ( 'NONE', #4696, 5.000000000000000000 ) ;
#8288 = CARTESIAN_POINT ( 'NONE',  ( 4.126438786023406635, -120.8149455287847758, 3.030370511718414317 ) ) ;
#8289 = CARTESIAN_POINT ( 'NONE',  ( 38.79999999999999716, 101.5999999999999943, 0.5000000000000000000 ) ) ;
#8290 = ORIENTED_EDGE ( 'NONE', *, *, #12107, .F. ) ;
#8291 = AXIS2_PLACEMENT_3D ( 'NONE', #1345, #12158, #178 ) ;
#8292 = B_SPLINE_CURVE_WITH_KNOTS ( 'NONE', 3,
 ( #6947, #1759, #10181, #7938, #10321, #7859, #4785, #9062, #2534, #5760, #8081, #10038, #12145, #4705 ),
 .UNSPECIFIED., .F., .F.,
 ( 4, 2, 2, 2, 2, 2, 4 ),
 ( 0.000000000000000000, 0.0003997920717328745199, 0.0007995841434657493651, 0.001199376215198624156, 0.001599168286931499164, 0.002398752430397248312, 0.003198336573862998328 ),
 .UNSPECIFIED. ) ;
#8293 = VECTOR ( 'NONE', #3492, 1000.000000000000000 ) ;
#8294 = EDGE_LOOP ( 'NONE', ( #431, #6025, #13849, #1199 ) ) ;
#8295 = FACE_BOUND ( 'NONE', #5735, .T. ) ;
#8296 = VERTEX_POINT ( 'NONE', #3238 ) ;
#8297 = CARTESIAN_POINT ( 'NONE',  ( -24.37649275748776390, -100.0000000000000000, -7.500000000000000000 ) ) ;
#8298 = CIRCLE ( 'NONE', #2239, 2.000000000000000000 ) ;
#8299 = DIRECTION ( 'NONE',  ( 1.000000000000000000, 0.000000000000000000, 0.000000000000000000 ) ) ;
#8300 = CARTESIAN_POINT ( 'NONE',  ( 6.383362303552328143, -84.46817857652109751, -7.102163859751367880 ) ) ;
#8301 = CIRCLE ( 'NONE', #3360, 4.999999999999997335 ) ;
#8302 = CARTESIAN_POINT ( 'NONE',  ( 41.49999999999999289, 98.00000000000001421, 7.500000000000000000 ) ) ;
#8303 = VECTOR ( 'NONE', #5182, 1000.000000000000000 ) ;
#8304 = DIRECTION ( 'NONE',  ( 0.000000000000000000, 0.000000000000000000, 1.000000000000000000 ) ) ;
#8305 = CARTESIAN_POINT ( 'NONE',  ( 10.29982004912477578, -6.336490384724132952, -1.734723475976807094E-15 ) ) ;
#8306 = DIRECTION ( 'NONE',  ( 0.9960067511297463483, -0.08927794634716619548, 0.000000000000000000 ) ) ;
#8307 = DIRECTION ( 'NONE',  ( -2.797435172181481150E-17, 1.000000000000000000, -1.765856845898762549E-18 ) ) ;
#8308 = EDGE_CURVE ( 'NONE', #5091, #4998, #3139, .T. ) ;
#8309 = DIRECTION ( 'NONE',  ( -0.7999999999999996003, -0.6000000000000007550, -8.673617379884038430E-16 ) ) ;
#8310 = CARTESIAN_POINT ( 'NONE',  ( 8.385254915620292238, -3.520109059331727241, 1.035430912652128846E-15 ) ) ;
#8311 = COLOUR_RGB ( '', 0.40784314, 0.44705882, 0.49803922) ;
#8312 = DIRECTION ( 'NONE',  ( -1.000000000000000000, 0.000000000000000000, 0.000000000000000000 ) ) ;
#8313 = AXIS2_PLACEMENT_3D ( 'NONE', #4180, #770, #4971 ) ;
#8314 = VERTEX_POINT ( 'NONE', #5144 ) ;
#8315 = CIRCLE ( 'NONE', #5618, 8.385254915620292238 ) ;
#8316 = DIRECTION ( 'NONE',  ( -0.000000000000000000, -0.000000000000000000, -1.000000000000000000 ) ) ;
#8317 = VERTEX_POINT ( 'NONE', #11463 ) ;
#8318 = DIRECTION ( 'NONE',  ( -0.9960067511297463483, 0.08927794634716618161, -4.818676322152979407E-17 ) ) ;
#8319 = EDGE_LOOP ( 'NONE', ( #10838, #8557, #3115, #355, #4837 ) ) ;
#8320 = CARTESIAN_POINT ( 'NONE',  ( -32.50000000000000000, 110.0000000000000142, -2.499999999999999556 ) ) ;
#8321 = DIRECTION ( 'NONE',  ( 0.000000000000000000, 0.000000000000000000, 1.000000000000000000 ) ) ;
#8322 = CARTESIAN_POINT ( 'NONE',  ( 3.628753873946515718, -79.03030303033179393, 9.983370075670988442 ) ) ;
#8323 = CARTESIAN_POINT ( 'NONE',  ( 20.16774360776483732, -62.63636365604191525, -2.887214122427654406 ) ) ;
#8324 = CIRCLE ( 'NONE', #726, 8.385254915620294014 ) ;
#8325 = EDGE_CURVE ( 'NONE', #576, #5704, #1144, .T. ) ;
#8326 = CARTESIAN_POINT ( 'NONE',  ( -29.00000000000000355, -3.551475717527324818E-15, 7.500000000000000000 ) ) ;
#8327 = EDGE_CURVE ( 'NONE', #2969, #11439, #10754, .T. ) ;
#8328 = EDGE_CURVE ( 'NONE', #9552, #2984, #13026, .T. ) ;
#8329 = DIRECTION ( 'NONE',  ( -0.000000000000000000, -0.000000000000000000, -1.000000000000000000 ) ) ;
#8330 = DIRECTION ( 'NONE',  ( 0.6000000000000001998, 0.7999999999999998224, -0.000000000000000000 ) ) ;
#8331 = EDGE_CURVE ( 'NONE', #8182, #30, #6970, .T. ) ;
#8332 = ADVANCED_FACE ( 'NONE', ( #9498 ), #8010, .T. ) ;
#8333 = ORIENTED_EDGE ( 'NONE', *, *, #12378, .T. ) ;
#8334 = AXIS2_PLACEMENT_3D ( 'NONE', #12197, #7915, #13200 ) ;
#8335 = ORIENTED_EDGE ( 'NONE', *, *, #4187, .F. ) ;
#8336 = DIRECTION ( 'NONE',  ( 0.000000000000000000, 0.000000000000000000, 1.000000000000000000 ) ) ;
#8337 = CARTESIAN_POINT ( 'NONE',  ( -15.29705854078138927, 66.79670324143890525, -2.109256209238486313E-15 ) ) ;
#8338 = CARTESIAN_POINT ( 'NONE',  ( 25.00000000000000355, 120.0000000000000284, -0.5000000000000000000 ) ) ;
#8339 = CARTESIAN_POINT ( 'NONE',  ( 8.385254915620292238, 69.25350232273815720, 9.022884433393300556E-16 ) ) ;
#8340 = CARTESIAN_POINT ( 'NONE',  ( -1.620286128678860127, -125.1459947693864194, -4.334625215706721768 ) ) ;
#8341 = CARTESIAN_POINT ( 'NONE',  ( -12.99553232110413425, 48.77386654458962312, -25.99106464220827917 ) ) ;
#8342 = ORIENTED_EDGE ( 'NONE', *, *, #10547, .T. ) ;
#8343 = EDGE_CURVE ( 'NONE', #10920, #4208, #4499, .T. ) ;
#8344 = VERTEX_POINT ( 'NONE', #6748 ) ;
#8345 = CIRCLE ( 'NONE', #11914, 22.99999999999999289 ) ;
#8346 = CIRCLE ( 'NONE', #2983, 5.999999999999998224 ) ;
#8347 = ORIENTED_EDGE ( 'NONE', *, *, #10772, .T. ) ;
#8348 = DIRECTION ( 'NONE',  ( 1.000000000000000000, 0.000000000000000000, 0.000000000000000000 ) ) ;
#8349 = VERTEX_POINT ( 'NONE', #8639 ) ;
#8350 = CARTESIAN_POINT ( 'NONE',  ( -12.97449437267216865, -39.59556244224027211, -25.94898874534435151 ) ) ;
#8351 = ORIENTED_EDGE ( 'NONE', *, *, #6708, .F. ) ;
#8352 = CARTESIAN_POINT ( 'NONE',  ( 10.69346802281034492, 11.89973432371241380, 0.000000000000000000 ) ) ;
#8353 = CARTESIAN_POINT ( 'NONE',  ( 30.29366116764611760, 20.61262658154624816, 2.500000000000005329 ) ) ;
#8354 = DIRECTION ( 'NONE',  ( 0.8035603370713739757, -0.5952233065713573579, 0.000000000000000000 ) ) ;
#8355 = DIRECTION ( 'NONE',  ( 0.000000000000000000, 0.000000000000000000, -1.000000000000000000 ) ) ;
#8356 = AXIS2_PLACEMENT_3D ( 'NONE', #12759, #3073, #2022 ) ;
#8357 = CARTESIAN_POINT ( 'NONE',  ( -2.861434295120944160, -135.9613303536295348, 1.766772280313772203 ) ) ;
#8358 = LINE ( 'NONE', #4076, #3253 ) ;
#8359 = ORIENTED_EDGE ( 'NONE', *, *, #3093, .T. ) ;
#8360 = EDGE_CURVE ( 'NONE', #4722, #7675, #1361, .T. ) ;
#8361 = VERTEX_POINT ( 'NONE', #240 ) ;
#8362 = EDGE_LOOP ( 'NONE', ( #4807, #3855, #622, #679 ) ) ;
#8363 = VECTOR ( 'NONE', #7226, 1000.000000000000000 ) ;
#8364 = CARTESIAN_POINT ( 'NONE',  ( 15.29705854078138572, 38.52236939141059935, 3.746698755667520834E-15 ) ) ;
#8365 = ORIENTED_EDGE ( 'NONE', *, *, #11757, .T. ) ;
#8366 = FACE_OUTER_BOUND ( 'NONE', #1632, .T. ) ;
#8367 = CARTESIAN_POINT ( 'NONE',  ( 8.845718597664788518, -89.07293163041987327, -1.670562313001050292 ) ) ;
#8368 = CARTESIAN_POINT ( 'NONE',  ( 12.97449437267217753, -39.59556244224027211, 0.000000000000000000 ) ) ;
#8369 = CARTESIAN_POINT ( 'NONE',  ( -2.517691654963332357E-15, 90.00000000000000000, -1.589271161308885878E-16 ) ) ;
#8370 = DIRECTION ( 'NONE',  ( 0.000000000000000000, 1.000000000000000000, 1.734723475976805615E-16 ) ) ;
#8371 = CIRCLE ( 'NONE', #86, 9.000000000009000800 ) ;
#8372 = DIRECTION ( 'NONE',  ( 0.9960067511297464593, -0.08927794634716622324, 3.401418580343279473E-17 ) ) ;
#8373 = FACE_OUTER_BOUND ( 'NONE', #7439, .T. ) ;
#8374 = VECTOR ( 'NONE', #312, 1000.000000000000000 ) ;
#8375 = ORIENTED_EDGE ( 'NONE', *, *, #10885, .T. ) ;
#8376 = CARTESIAN_POINT ( 'NONE',  ( 47.69307742500824787, -16.90904448151677286, -2.500000000000002665 ) ) ;
#8377 = DIRECTION ( 'NONE',  ( 0.000000000000000000, 0.000000000000000000, 1.000000000000000000 ) ) ;
#8378 = CARTESIAN_POINT ( 'NONE',  ( 0.1916457366472302803, -105.1818181818151317, 4.609965990740150232 ) ) ;
#8379 = ORIENTED_EDGE ( 'NONE', *, *, #12704, .T. ) ;
#8380 = EDGE_CURVE ( 'NONE', #11850, #6243, #13510, .T. ) ;
#8381 = CARTESIAN_POINT ( 'NONE',  ( 35.00000000000000000, 4.286263797015736496E-15, 4.000000000000000000 ) ) ;
#8382 = VERTEX_POINT ( 'NONE', #8927 ) ;
#8383 = AXIS2_PLACEMENT_3D ( 'NONE', #6881, #11159, #13374 ) ;
#8384 = LINE ( 'NONE', #118, #5043 ) ;
#8385 = DIRECTION ( 'NONE',  ( -6.158143864569485777E-17, -2.736152283717910599E-16, 1.000000000000000000 ) ) ;
#8386 = CARTESIAN_POINT ( 'NONE',  ( 0.000000000000000000, 40.00000000000000000, 0.000000000000000000 ) ) ;
#8387 = CARTESIAN_POINT ( 'NONE',  ( -60.00000000000001421, 20.00000000000000000, -4.000000000000000000 ) ) ;
#8388 = CARTESIAN_POINT ( 'NONE',  ( 25.00000000000000355, 120.0000000000000284, 2.500000000000000000 ) ) ;
#8389 = DIRECTION ( 'NONE',  ( -6.158143864569485777E-17, -2.736152283717910599E-16, 1.000000000000000000 ) ) ;
#8390 = CYLINDRICAL_SURFACE ( 'NONE', #7909, 15.29705854078139460 ) ;
#8391 = AXIS2_PLACEMENT_3D ( 'NONE', #3539, #6780, #12186 ) ;
#8392 = CARTESIAN_POINT ( 'NONE',  ( 11.81226048336477064, -40.00941361824966691, 2.893169398329486201E-15 ) ) ;
#8393 = AXIS2_PLACEMENT_3D ( 'NONE', #1167, #5424, #5160 ) ;
#8394 = ORIENTED_EDGE ( 'NONE', *, *, #4368, .F. ) ;
#8395 = CIRCLE ( 'NONE', #2338, 5.000000000000000000 ) ;
#8396 = ADVANCED_FACE ( 'NONE', ( #1275 ), #174, .F. ) ;
#8397 = EDGE_CURVE ( 'NONE', #9893, #6779, #6295, .T. ) ;
#8398 = VERTEX_POINT ( 'NONE', #13231 ) ;
#8399 = EDGE_CURVE ( 'NONE', #5520, #9444, #5412, .T. ) ;
#8400 = DIRECTION ( 'NONE',  ( -0.000000000000000000, -0.000000000000000000, -1.000000000000000000 ) ) ;
#8401 = CIRCLE ( 'NONE', #4143, 18.74900000001875000 ) ;
#8402 = CARTESIAN_POINT ( 'NONE',  ( -15.29705854078139282, 66.79670324143890525, 30.59411708156276788 ) ) ;
#8403 = AXIS2_PLACEMENT_3D ( 'NONE', #31, #7370, #7241 ) ;
#8404 = DIRECTION ( 'NONE',  ( -1.000000000000000000, 0.000000000000000000, 0.000000000000000000 ) ) ;
#8405 = CARTESIAN_POINT ( 'NONE',  ( 2.615685906363557134, -134.4805512794541187, -2.371495061727838305 ) ) ;
#8406 = DIRECTION ( 'NONE',  ( 0.5753203450992270263, 0.8179281756455796248, 2.409338161076488717E-16 ) ) ;
#8407 = VERTEX_POINT ( 'NONE', #9695 ) ;
#8408 = ORIENTED_EDGE ( 'NONE', *, *, #13664, .T. ) ;
#8409 = CIRCLE ( 'NONE', #2819, 8.385254915620292238 ) ;
#8410 = ADVANCED_FACE ( 'NONE', ( #8777 ), #4420, .T. ) ;
#8411 = CARTESIAN_POINT ( 'NONE',  ( -42.16244658108818300, 105.4500712252157655, -2.499999999999999556 ) ) ;
#8412 = PRESENTATION_LAYER_ASSIGNMENT (  '', '', ( #5507 ) ) ;
#8413 = EDGE_CURVE ( 'NONE', #6698, #8935, #4355, .T. ) ;
#8414 = AXIS2_PLACEMENT_3D ( 'NONE', #1703, #7870, #4793 ) ;
#8415 = CARTESIAN_POINT ( 'NONE',  ( 33.39358510189354945, -25.44935030951552690, -2.500000000000006217 ) ) ;
#8416 = ORIENTED_EDGE ( 'NONE', *, *, #7138, .T. ) ;
#8417 = DIRECTION ( 'NONE',  ( -0.000000000000000000, -0.000000000000000000, -1.000000000000000000 ) ) ;
#8418 = EDGE_LOOP ( 'NONE', ( #13681, #1372 ) ) ;
#8419 = EDGE_CURVE ( 'NONE', #13516, #283, #10984, .T. ) ;
#8420 = CARTESIAN_POINT ( 'NONE',  ( 8.385254915620292238, 5.904668890677672088, 1.018788103988028800E-15 ) ) ;
#8421 = ADVANCED_FACE ( 'NONE', ( #8704 ), #2037, .F. ) ;
#8422 = LINE ( 'NONE', #856, #2656 ) ;
#8423 = AXIS2_PLACEMENT_3D ( 'NONE', #11683, #711, #3784 ) ;
#8424 = CARTESIAN_POINT ( 'NONE',  ( -13.79311422413708499, -21.62638421600851046, -7.500000000000000000 ) ) ;
#8425 = CARTESIAN_POINT ( 'NONE',  ( 14.53672965213156942, 15.21527412409548674, 2.500000000000003109 ) ) ;
#8426 = CARTESIAN_POINT ( 'NONE',  ( -12.99553232110414491, -17.19957910547634228, -1.530749717005650972E-15 ) ) ;
#8427 = CARTESIAN_POINT ( 'NONE',  ( 4.459053427763567612, -109.9755374418222829, -4.679063774435563872 ) ) ;
#8428 = CARTESIAN_POINT ( 'NONE',  ( 34.99999999999958789, 1.063887963769481123E-13, 12.50000000000000000 ) ) ;
#8429 = EDGE_LOOP ( 'NONE', ( #7799, #823, #7488, #9740, #4776, #6443 ) ) ;
#8430 = ORIENTED_EDGE ( 'NONE', *, *, #4296, .F. ) ;
#8431 = EDGE_CURVE ( 'NONE', #6547, #3108, #7407, .T. ) ;
#8432 = B_SPLINE_CURVE_WITH_KNOTS ( 'NONE', 3,
 ( #238, #11931, #6667, #7654 ),
 .UNSPECIFIED., .F., .F.,
 ( 4, 4 ),
 ( 0.000000000000000000, 1.000000000000000000 ),
 .UNSPECIFIED. ) ;
#8433 = CARTESIAN_POINT ( 'NONE',  ( -8.385254915620297567, 40.97916847270985841, 16.77050983124058448 ) ) ;
#8434 = CARTESIAN_POINT ( 'NONE',  ( 1.493586498966360088, -80.00119264582536971, 9.937293197986129201 ) ) ;
#8435 = CARTESIAN_POINT ( 'NONE',  ( 10.69346802281034847, 40.17406817374067174, -21.38693604562068984 ) ) ;
#8436 = CARTESIAN_POINT ( 'NONE',  ( 8.747338040274810211, -91.10717937812032119, 0.8989578942604090628 ) ) ;
#8437 = EDGE_CURVE ( 'NONE', #13647, #5607, #13663, .T. ) ;
#8438 = CARTESIAN_POINT ( 'NONE',  ( -8.385254915620292238, 62.45333659073423860, -2.210618003686766271E-15 ) ) ;
#8439 = CARTESIAN_POINT ( 'NONE',  ( 12.99553232110414136, 20.49953269456136695, 1.563396152262992288E-15 ) ) ;
#8440 = CARTESIAN_POINT ( 'NONE',  ( 15.29705854078139815, 0.8232575913729167638, -30.59411708156277854 ) ) ;
#8441 = AXIS2_PLACEMENT_3D ( 'NONE', #66, #7682, #1180 ) ;
#8442 = DIRECTION ( 'NONE',  ( -0.000000000000000000, -0.000000000000000000, -1.000000000000000000 ) ) ;
#8443 = FACE_OUTER_BOUND ( 'NONE', #8987, .T. ) ;
#8444 = CARTESIAN_POINT ( 'NONE',  ( -35.00000000000000000, -4.286263797015736496E-15, 7.500000000000000000 ) ) ;
#8445 = DIRECTION ( 'NONE',  ( 0.9960067511297463483, -0.08927794634716618161, 4.818676322152979407E-17 ) ) ;
#8446 = DIRECTION ( 'NONE',  ( 0.000000000000000000, 0.000000000000000000, 1.000000000000000000 ) ) ;
#8447 = CARTESIAN_POINT ( 'NONE',  ( -8.943257790340283009, -76.35064935061960512, -10.27353203466038423 ) ) ;
#8448 = ORIENTED_EDGE ( 'NONE', *, *, #2410, .F. ) ;
#8449 = DIRECTION ( 'NONE',  ( -2.797435172181481150E-17, 1.000000000000000000, -1.765856845898762549E-18 ) ) ;
#8450 = VERTEX_POINT ( 'NONE', #7787 ) ;
#8451 = DIRECTION ( 'NONE',  ( -0.000000000000000000, -0.000000000000000000, -1.000000000000000000 ) ) ;
#8452 = CARTESIAN_POINT ( 'NONE',  ( 25.00000000000000355, 120.0000000000000142, 2.500000000000000000 ) ) ;
#8453 = CARTESIAN_POINT ( 'NONE',  ( 41.50000000000000711, 98.00000000000000000, -2.499999999999999556 ) ) ;
#8454 = CARTESIAN_POINT ( 'NONE',  ( 2.937342332081942953, -95.36363636365133800, 3.570487953802512049 ) ) ;
#8455 = LINE ( 'NONE', #11681, #2243 ) ;
#8456 = CARTESIAN_POINT ( 'NONE',  ( 14.99223790936468603, -6.835163196276449860, -2.500000000000002665 ) ) ;
#8457 = CARTESIAN_POINT ( 'NONE',  ( 32.50000000000000000, 4.286263797015736496E-15, 7.500000000000000000 ) ) ;
#8458 = CARTESIAN_POINT ( 'NONE',  ( -1.219787497442949287E-15, 43.60378069071538221, -7.699803463976802609E-17 ) ) ;
#8459 = DIRECTION ( 'NONE',  ( -0.1234677578012386562, -1.701584941912606716E-18, 0.9923485843107423543 ) ) ;
#8460 = ORIENTED_EDGE ( 'NONE', *, *, #12173, .F. ) ;
#8461 = CIRCLE ( 'NONE', #1302, 15.29705854078139993 ) ;
#8462 = VERTEX_POINT ( 'NONE', #5989 ) ;
#8463 = FACE_OUTER_BOUND ( 'NONE', #3033, .T. ) ;
#8464 = CARTESIAN_POINT ( 'NONE',  ( 10.69346802281033959, 68.44840202376897764, 21.38693604562069339 ) ) ;
#8465 = CARTESIAN_POINT ( 'NONE',  ( 34.28542361028948449, 108.1059200568371068, 1.103255912984089537 ) ) ;
#8466 = LINE ( 'NONE', #7417, #5163 ) ;
#8467 = FACE_OUTER_BOUND ( 'NONE', #3200, .T. ) ;
#8468 = EDGE_CURVE ( 'NONE', #13392, #9123, #11160, .T. ) ;
#8469 = FACE_OUTER_BOUND ( 'NONE', #4033, .T. ) ;
#8470 = AXIS2_PLACEMENT_3D ( 'NONE', #10023, #2738, #4690 ) ;
#8471 = ORIENTED_EDGE ( 'NONE', *, *, #2528, .T. ) ;
#8472 = ORIENTED_EDGE ( 'NONE', *, *, #2616, .F. ) ;
#8473 = ORIENTED_EDGE ( 'NONE', *, *, #8155, .T. ) ;
#8474 = CARTESIAN_POINT ( 'NONE',  ( 10.00000000000000000, 90.00000000000000000, 2.500000000000000000 ) ) ;
#8475 = CARTESIAN_POINT ( 'NONE',  ( -2.179449471770338320, 90.00000000000000000, -4.500000000000000888 ) ) ;
#8476 = AXIS2_PLACEMENT_3D ( 'NONE', #7604, #10627, #2141 ) ;
#8477 = ORIENTED_EDGE ( 'NONE', *, *, #13139, .T. ) ;
#8478 = CARTESIAN_POINT ( 'NONE',  ( 12.97449437267218109, -39.59556244224027211, -25.94898874534434086 ) ) ;
#8479 = ORIENTED_EDGE ( 'NONE', *, *, #7873, .T. ) ;
#8480 = DIRECTION ( 'NONE',  ( 1.000000000000000000, 0.000000000000000000, 0.000000000000000000 ) ) ;
#8481 = CARTESIAN_POINT ( 'NONE',  ( -1.341290363786561812E-15, 47.94714734142005597, -8.466779837416320124E-17 ) ) ;
#8482 = CARTESIAN_POINT ( 'NONE',  ( -8.385254915620292238, 15.32944684068712782, -2.706960864746847057E-17 ) ) ;
#8483 = DIRECTION ( 'NONE',  ( -1.000000000000000000, -2.835060530349835421E-17, 0.000000000000000000 ) ) ;
#8484 = CARTESIAN_POINT ( 'NONE',  ( -8.385254915620294014, -15.56949922734665570, 2.749350679782564022E-17 ) ) ;
#8485 = ADVANCED_FACE ( 'NONE', ( #2543 ), #13386, .T. ) ;
#8486 = CARTESIAN_POINT ( 'NONE',  ( -0.7710117948378325536, -151.5922553772190895, -1.650848015692418569 ) ) ;
#8487 = EDGE_CURVE ( 'NONE', #13048, #10681, #2654, .T. ) ;
#8488 = CARTESIAN_POINT ( 'NONE',  ( -35.00000000000000711, -25.00000000000000711, 7.500000000000000000 ) ) ;
#8489 = EDGE_CURVE ( 'NONE', #4145, #4671, #2686, .T. ) ;
#8490 = ORIENTED_EDGE ( 'NONE', *, *, #12699, .F. ) ;
#8491 = CARTESIAN_POINT ( 'NONE',  ( 62.16766351966359849, -73.17985663200910551, -2.500000000000000000 ) ) ;
#8492 = EDGE_LOOP ( 'NONE', ( #6566, #12774, #9156, #4327, #3927, #2242, #11068, #1330 ) ) ;
#8493 = EDGE_CURVE ( 'NONE', #11251, #11452, #3989, .T. ) ;
#8494 = EDGE_CURVE ( 'NONE', #8894, #1175, #11388, .T. ) ;
#8495 = CIRCLE ( 'NONE', #10723, 5.000000000000000000 ) ;
#8496 = CARTESIAN_POINT ( 'NONE',  ( -10.69346802281034670, 40.17406817374066463, -1.451455445216333422E-15 ) ) ;
#8497 = DIRECTION ( 'NONE',  ( -0.9960067511297463483, 0.08927794634716618161, -4.818676322152979407E-17 ) ) ;
#8498 = CARTESIAN_POINT ( 'NONE',  ( -3.034625339109073394, -118.9865377956984389, -4.388674898262355129 ) ) ;
#8499 = CARTESIAN_POINT ( 'NONE',  ( -12.99553232110413781, -7.774801155466916747, -25.99106464220828627 ) ) ;
#8500 = VECTOR ( 'NONE', #1011, 1000.000000000000000 ) ;
#8501 = DIRECTION ( 'NONE',  ( -2.797435172181481150E-17, 1.000000000000000000, -1.765856845898762549E-18 ) ) ;
#8502 = DIRECTION ( 'NONE',  ( 0.000000000000000000, 0.000000000000000000, -1.000000000000000000 ) ) ;
#8503 = AXIS2_PLACEMENT_3D ( 'NONE', #10743, #3444, #12009 ) ;
#8504 = FACE_OUTER_BOUND ( 'NONE', #13415, .T. ) ;
#8505 = AXIS2_PLACEMENT_3D ( 'NONE', #3414, #2438, #6446 ) ;
#8506 = DIRECTION ( 'NONE',  ( 1.000000000000000000, 0.000000000000000000, 0.000000000000000000 ) ) ;
#8507 = CARTESIAN_POINT ( 'NONE',  ( -10.00000000000000711, 139.9999999999999716, -0.5000000000000000000 ) ) ;
#8508 =( BOUNDED_SURFACE ( )  B_SPLINE_SURFACE ( 3, 3, ( 
 ( #1484, #12501, #13381, #8997 ),
 ( #13526, #12292, #3731, #10324 ),
 ( #3865, #2682, #11367, #6050 ),
 ( #6251, #1904, #5121, #11443 ) ),
 .UNSPECIFIED., .F., .F., .T. ) 
 B_SPLINE_SURFACE_WITH_KNOTS ( ( 4, 4 ),
 ( 4, 4 ),
 ( 0.000000000000000000, 1.000000000000000000 ),
 ( 0.000000000000000000, 1.000000000000000000 ),
 .UNSPECIFIED. ) 
 GEOMETRIC_REPRESENTATION_ITEM ( )  RATIONAL_B_SPLINE_SURFACE ( (
 ( 1.000000000000000000, 0.3333333333333334259, 0.3333333333333334259, 1.000000000000000000),
 ( 1.000000000000000000, 0.3333333333333334259, 0.3333333333333334259, 1.000000000000000000),
 ( 1.000000000000000000, 0.3333333333333334259, 0.3333333333333334259, 1.000000000000000000),
 ( 1.000000000000000000, 0.3333333333333334259, 0.3333333333333334259, 1.000000000000000000) ) ) 
 REPRESENTATION_ITEM ( '' )  SURFACE ( )  );
#8509 = ORIENTED_EDGE ( 'NONE', *, *, #124, .F. ) ;
#8510 = EDGE_CURVE ( 'NONE', #1315, #10763, #4747, .T. ) ;
#8511 = CARTESIAN_POINT ( 'NONE',  ( 31.28009342530033265, 25.22721338310705264, 2.500000000000006661 ) ) ;
#8512 = MECHANICAL_DESIGN_GEOMETRIC_PRESENTATION_REPRESENTATION (  '', ( #12331 ), #7170 ) ;
#8513 = VERTEX_POINT ( 'NONE', #1701 ) ;
#8514 = ORIENTED_EDGE ( 'NONE', *, *, #2211, .F. ) ;
#8515 = VECTOR ( 'NONE', #11233, 1000.000000000000000 ) ;
#8516 = CARTESIAN_POINT ( 'NONE',  ( 15.29705854078139282, -10.48808792804187284, 3.746698755667523200E-15 ) ) ;
#8517 = ORIENTED_EDGE ( 'NONE', *, *, #5751, .F. ) ;
#8518 = LINE ( 'NONE', #9643, #5701 ) ;
#8519 = CARTESIAN_POINT ( 'NONE',  ( 1.387778780781445676E-14, -100.0000000000000000, 0.000000000000000000 ) ) ;
#8520 = CARTESIAN_POINT ( 'NONE',  ( 4.864544286455739552, -89.44155844152219004, 0.3495895964544955548 ) ) ;
#8521 =( GEOMETRIC_REPRESENTATION_CONTEXT ( 3 ) GLOBAL_UNCERTAINTY_ASSIGNED_CONTEXT ( ( #1524 ) ) GLOBAL_UNIT_ASSIGNED_CONTEXT ( ( #2490, #6842, #11694 ) ) REPRESENTATION_CONTEXT ( 'NONE', 'WORKASPACE' ) );
#8522 = DIRECTION ( 'NONE',  ( -0.000000000000000000, -0.000000000000000000, -1.000000000000000000 ) ) ;
#8523 = FACE_OUTER_BOUND ( 'NONE', #862, .T. ) ;
#8524 = LINE ( 'NONE', #12827, #2146 ) ;
#8525 = AXIS2_PLACEMENT_3D ( 'NONE', #8613, #1316, #1190 ) ;
#8526 = CARTESIAN_POINT ( 'NONE',  ( 34.99999999999958789, 1.104930248025249758E-13, -2.499999999999999112 ) ) ;
#8527 = LINE ( 'NONE', #4174, #11829 ) ;
#8528 = ADVANCED_FACE ( 'NONE', ( #10121 ), #730, .T. ) ;
#8529 = ORIENTED_EDGE ( 'NONE', *, *, #354, .T. ) ;
#8530 =( BOUNDED_SURFACE ( )  B_SPLINE_SURFACE ( 3, 3, ( 
 ( #13001, #3368, #2383, #11926 ),
 ( #305, #6663, #9825, #4492 ),
 ( #10932, #4559, #1333, #5616 ),
 ( #8839, #13149, #4707, #8993 ) ),
 .UNSPECIFIED., .F., .F., .F. ) 
 B_SPLINE_SURFACE_WITH_KNOTS ( ( 4, 4 ),
 ( 4, 4 ),
 ( 0.000000000000000000, 1.000000000000000000 ),
 ( 0.000000000000000000, 1.000000000000000000 ),
 .UNSPECIFIED. ) 
 GEOMETRIC_REPRESENTATION_ITEM ( )  RATIONAL_B_SPLINE_SURFACE ( (
 ( 1.000000000000000000, 0.3333333333333334259, 0.3333333333333334259, 1.000000000000000000),
 ( 1.000000000000000000, 0.3333333333333334259, 0.3333333333333334259, 1.000000000000000000),
 ( 1.000000000000000000, 0.3333333333333334259, 0.3333333333333334259, 1.000000000000000000),
 ( 1.000000000000000000, 0.3333333333333334259, 0.3333333333333334259, 1.000000000000000000) ) ) 
 REPRESENTATION_ITEM ( '' )  SURFACE ( )  );
#8531 = CIRCLE ( 'NONE', #1606, 9.000000000008999024 ) ;
#8532 = VECTOR ( 'NONE', #3380, 1000.000000000000000 ) ;
#8533 =( LENGTH_UNIT ( ) NAMED_UNIT ( * ) SI_UNIT ( .MILLI., .METRE. ) );
#8534 = ORIENTED_EDGE ( 'NONE', *, *, #1984, .T. ) ;
#8535 = CARTESIAN_POINT ( 'NONE',  ( -15.29705854078139282, 55.48535772202409078, -9.797919878057798703E-17 ) ) ;
#8536 = FACE_OUTER_BOUND ( 'NONE', #956, .T. ) ;
#8537 = CARTESIAN_POINT ( 'NONE',  ( 10.69381717166375445, 53.83378072214353693, 2.619229793989003951E-15 ) ) ;
#8538 = CARTESIAN_POINT ( 'NONE',  ( -0.7998255503467009975, -126.5099019064922743, -4.384466114569518957 ) ) ;
#8539 = CYLINDRICAL_SURFACE ( 'NONE', #9386, 8.385254915620294014 ) ;
#8540 = ORIENTED_EDGE ( 'NONE', *, *, #5677, .F. ) ;
#8541 = PRODUCT_DEFINITION_SHAPE ( 'NONE', 'NONE',  #13902 ) ;
#8542 = CIRCLE ( 'NONE', #2951, 9.000000000008999024 ) ;
#8543 = ORIENTED_EDGE ( 'NONE', *, *, #13758, .F. ) ;
#8544 = EDGE_CURVE ( 'NONE', #2431, #9931, #5712, .T. ) ;
#8545 = VERTEX_POINT ( 'NONE', #2757 ) ;
#8546 = VERTEX_POINT ( 'NONE', #6958 ) ;
#8547 = CARTESIAN_POINT ( 'NONE',  ( 15.29705854078138749, 74.33491362204296138, 30.59411708156278564 ) ) ;
#8548 = VECTOR ( 'NONE', #5214, 1000.000000000000000 ) ;
#8549 = CYLINDRICAL_SURFACE ( 'NONE', #2875, 4.999999999999998224 ) ;
#8550 = PRESENTATION_STYLE_ASSIGNMENT (( #8822 ) ) ;
#8551 = DIRECTION ( 'NONE',  ( 0.1234677578012386562, 1.701584941912606716E-18, -0.9923485843107423543 ) ) ;
#8552 = DIRECTION ( 'NONE',  ( 0.000000000000000000, 1.000000000000000000, -0.000000000000000000 ) ) ;
#8553 = CARTESIAN_POINT ( 'NONE',  ( -10.69381717166375623, 63.25855867215299355, -1.533026014780321478E-15 ) ) ;
#8554 = DIRECTION ( 'NONE',  ( -0.000000000000000000, -0.000000000000000000, -1.000000000000000000 ) ) ;
#8555 = EDGE_LOOP ( 'NONE', ( #940, #12556, #6847, #8598 ) ) ;
#8556 = ORIENTED_EDGE ( 'NONE', *, *, #4364, .T. ) ;
#8557 = ORIENTED_EDGE ( 'NONE', *, *, #3773, .T. ) ;
#8558 = EDGE_CURVE ( 'NONE', #7842, #4998, #2199, .T. ) ;
#8559 = CARTESIAN_POINT ( 'NONE',  ( -2.179449471770338320, 90.00000000000000000, 4.500000000000000888 ) ) ;
#8560 = ADVANCED_FACE ( 'NONE', ( #10187 ), #5109, .T. ) ;
#8561 = ORIENTED_EDGE ( 'NONE', *, *, #6019, .T. ) ;
#8562 = LINE ( 'NONE', #10794, #754 ) ;
#8563 = CARTESIAN_POINT ( 'NONE',  ( 23.75221630157310315, -98.98132178242397572, -7.500000000000000000 ) ) ;
#8564 = CARTESIAN_POINT ( 'NONE',  ( 6.895584828341370986, -94.56397396217489870, 4.654405414161209897 ) ) ;
#8565 = LINE ( 'NONE', #95, #5813 ) ;
#8566 = AXIS2_PLACEMENT_3D ( 'NONE', #5178, #13775, #12695 ) ;
#8567 = CARTESIAN_POINT ( 'NONE',  ( 0.3134609018104931866, -154.2164502171992240, -0.8036717672280221381 ) ) ;
#8568 = DIRECTION ( 'NONE',  ( -6.158143864569485777E-17, -2.736152283717910599E-16, 1.000000000000000000 ) ) ;
#8569 = DIRECTION ( 'NONE',  ( 1.000000000000000000, 2.775557561562892929E-15, 0.000000000000000000 ) ) ;
#8570 = EDGE_CURVE ( 'NONE', #5648, #1545, #4926, .T. ) ;
#8571 = AXIS2_PLACEMENT_3D ( 'NONE', #1875, #13631, #5100 ) ;
#8572 = DIRECTION ( 'NONE',  ( 0.8907235428302465730, -0.4545454545454549189, 0.000000000000000000 ) ) ;
#8573 = ADVANCED_FACE ( 'NONE', ( #8090 ), #7026, .T. ) ;
#8574 = CARTESIAN_POINT ( 'NONE',  ( 1.024078386997840262, -80.66666666666725405, -9.976024522090996882 ) ) ;
#8575 = DIRECTION ( 'NONE',  ( -1.000000000000000000, 0.000000000000000000, 0.000000000000000000 ) ) ;
#8576 = CARTESIAN_POINT ( 'NONE',  ( 10.00000000000000000, 99.99999999999994316, 2.500000000000000000 ) ) ;
#8577 = VECTOR ( 'NONE', #5256, 1000.000000000000000 ) ;
#8578 = ORIENTED_EDGE ( 'NONE', *, *, #9954, .T. ) ;
#8579 = CARTESIAN_POINT ( 'NONE',  ( 56.05919550416194141, -1.881564379087037553, -2.499999999999998224 ) ) ;
#8580 = AXIS2_PLACEMENT_3D ( 'NONE', #11711, #6453, #13477 ) ;
#8581 = EDGE_LOOP ( 'NONE', ( #4631, #12750, #5682, #8157, #11335 ) ) ;
#8582 = ORIENTED_EDGE ( 'NONE', *, *, #12359, .F. ) ;
#8583 = EDGE_CURVE ( 'NONE', #12700, #1806, #41, .T. ) ;
#8584 = CARTESIAN_POINT ( 'NONE',  ( -25.00000000000000355, 120.0000000000000284, -0.5000000000000000000 ) ) ;
#8585 = ORIENTED_EDGE ( 'NONE', *, *, #5395, .F. ) ;
#8586 = ORIENTED_EDGE ( 'NONE', *, *, #13434, .T. ) ;
#8587 = CYLINDRICAL_SURFACE ( 'NONE', #6368, 25.00000000000000711 ) ;
#8588 = FACE_OUTER_BOUND ( 'NONE', #13668, .T. ) ;
#8589 = EDGE_CURVE ( 'NONE', #6325, #6913, #12063, .T. ) ;
#8590 = CARTESIAN_POINT ( 'NONE',  ( 12.09338464843078675, -169.0000000000000000, -0.006909782850910250844 ) ) ;
#8591 = ADVANCED_FACE ( 'NONE', ( #4404 ), #12988, .F. ) ;
#8592 = FACE_OUTER_BOUND ( 'NONE', #12465, .T. ) ;
#8593 = CARTESIAN_POINT ( 'NONE',  ( 10.69346802281034847, 11.89973432371241202, -21.38693604562068629 ) ) ;
#8594 = DIRECTION ( 'NONE',  ( -1.000000000000000000, 0.000000000000000000, 0.000000000000000000 ) ) ;
#8595 = DIRECTION ( 'NONE',  ( -0.000000000000000000, -0.000000000000000000, -1.000000000000000000 ) ) ;
#8596 = VERTEX_POINT ( 'NONE', #19 ) ;
#8597 = CIRCLE ( 'NONE', #7033, 25.50000000002550138 ) ;
#8598 = ORIENTED_EDGE ( 'NONE', *, *, #1741, .F. ) ;
#8599 = CARTESIAN_POINT ( 'NONE',  ( -15.29705854078138749, 46.06057977201469100, -30.59411708156277854 ) ) ;
#8600 = LINE ( 'NONE', #8886, #13575 ) ;
#8601 = ADVANCED_FACE ( 'NONE', ( #10850 ), #5747, .T. ) ;
#8602 = AXIS2_PLACEMENT_3D ( 'NONE', #9063, #13379, #3728 ) ;
#8603 = DIRECTION ( 'NONE',  ( -0.000000000000000000, -0.000000000000000000, -1.000000000000000000 ) ) ;
#8604 = CARTESIAN_POINT ( 'NONE',  ( -19.84413750617685324, 26.75684992538831253, 2.573597559463546069 ) ) ;
#8605 = CARTESIAN_POINT ( 'NONE',  ( 22.42156014662059249, -97.00000000000000000, 7.500000000000000000 ) ) ;
#8606 = CARTESIAN_POINT ( 'NONE',  ( 8.385254915620292238, 90.00000000000000000, 8.679704431140118580E-16 ) ) ;
#8607 = ORIENTED_EDGE ( 'NONE', *, *, #9722, .F. ) ;
#8608 =( BOUNDED_SURFACE ( )  B_SPLINE_SURFACE ( 3, 3, ( 
 ( #13866, #8433, #5135, #7438 ),
 ( #8496, #9354, #9558, #2110 ),
 ( #13737, #7169, #11592, #12723 ),
 ( #12591, #1846, #6261, #8364 ) ),
 .UNSPECIFIED., .F., .F., .T. ) 
 B_SPLINE_SURFACE_WITH_KNOTS ( ( 4, 4 ),
 ( 4, 4 ),
 ( 0.000000000000000000, 1.000000000000000000 ),
 ( 0.000000000000000000, 1.000000000000000000 ),
 .UNSPECIFIED. ) 
 GEOMETRIC_REPRESENTATION_ITEM ( )  RATIONAL_B_SPLINE_SURFACE ( (
 ( 1.000000000000000000, 0.3333333333333334259, 0.3333333333333334259, 1.000000000000000000),
 ( 1.000000000000000000, 0.3333333333333334259, 0.3333333333333334259, 1.000000000000000000),
 ( 1.000000000000000000, 0.3333333333333334259, 0.3333333333333334259, 1.000000000000000000),
 ( 1.000000000000000000, 0.3333333333333334259, 0.3333333333333334259, 1.000000000000000000) ) ) 
 REPRESENTATION_ITEM ( '' )  SURFACE ( )  );
#8609 = VECTOR ( 'NONE', #1350, 1000.000000000000000 ) ;
#8610 = ORIENTED_EDGE ( 'NONE', *, *, #13336, .F. ) ;
#8611 = CIRCLE ( 'NONE', #12668, 25.00000000000000711 ) ;
#8612 = VERTEX_POINT ( 'NONE', #9122 ) ;
#8613 = CARTESIAN_POINT ( 'NONE',  ( -6.924833908958124424E-16, 24.75422479069652582, -4.371241731156832241E-17 ) ) ;
#8614 = FACE_OUTER_BOUND ( 'NONE', #12533, .T. ) ;
#8615 = CARTESIAN_POINT ( 'NONE',  ( -6.174202239351583188, -74.54647412380100491, -8.025911163902851087 ) ) ;
#8616 = DIRECTION ( 'NONE',  ( -1.000000000000000000, 0.000000000000000000, 0.000000000000000000 ) ) ;
#8617 = LINE ( 'NONE', #6583, #3884 ) ;
#8618 = CARTESIAN_POINT ( 'NONE',  ( -2.799701502495941963, -101.5643811721427738, -6.922737930671543971 ) ) ;
#8619 = CARTESIAN_POINT ( 'NONE',  ( -0.9875499244693202172, -80.00464164737402939, 10.06307371418729701 ) ) ;
#8620 = AXIS2_PLACEMENT_3D ( 'NONE', #2468, #11168, #1554 ) ;
#8621 = VERTEX_POINT ( 'NONE', #13366 ) ;
#8622 = EDGE_LOOP ( 'NONE', ( #8534, #3011, #6309, #13645 ) ) ;
#8623 = STYLED_ITEM ( 'NONE', ( #5473 ), #11412 ) ;
#8624 = ORIENTED_EDGE ( 'NONE', *, *, #190, .F. ) ;
#8625 = AXIS2_PLACEMENT_3D ( 'NONE', #7945, #1418, #5915 ) ;
#8626 = CARTESIAN_POINT ( 'NONE',  ( -3.629742700906668951, 90.29727615934677942, 3.441963681523289242 ) ) ;
#8627 = LINE ( 'NONE', #12932, #5154 ) ;
#8628 = ORIENTED_EDGE ( 'NONE', *, *, #11589, .T. ) ;
#8629 = CARTESIAN_POINT ( 'NONE',  ( -38.80000000000001137, 101.5999999999999943, 0.5000000000000000000 ) ) ;
#8630 = CIRCLE ( 'NONE', #7297, 5.000000000000000000 ) ;
#8631 = DIRECTION ( 'NONE',  ( -1.224646799147353207E-16, 1.000000000000000000, -0.000000000000000000 ) ) ;
#8632 = CARTESIAN_POINT ( 'NONE',  ( -12.99553232110414491, 1.649976794542511893, -1.597320951662050367E-15 ) ) ;
#8633 = CARTESIAN_POINT ( 'NONE',  ( -3.510313888878303423, -133.0909090908702126, 1.034921094667177410 ) ) ;
#8634 = DIRECTION ( 'NONE',  ( -0.000000000000000000, -0.000000000000000000, -1.000000000000000000 ) ) ;
#8635 = AXIS2_PLACEMENT_3D ( 'NONE', #12751, #7411, #8668 ) ;
#8636 = CARTESIAN_POINT ( 'NONE',  ( 0.2677229415529756018, -160.9696969707963774, -0.7106593571500791073 ) ) ;
#8637 = CIRCLE ( 'NONE', #11771, 15.29705854078139105 ) ;
#8638 = CARTESIAN_POINT ( 'NONE',  ( -7.500230552170997100, -73.18181818181757592, -6.960552780978341403 ) ) ;
#8639 = CARTESIAN_POINT ( 'NONE',  ( -13.79311422413708499, -20.00000000000000355, -7.500000000000000000 ) ) ;
#8640 = LINE ( 'NONE', #9697, #7468 ) ;
#8641 = EDGE_CURVE ( 'NONE', #7744, #12738, #13207, .T. ) ;
#8642 = ADVANCED_FACE ( 'NONE', ( #12137 ), #7184, .T. ) ;
#8643 = EDGE_LOOP ( 'NONE', ( #6011, #9237, #11112, #5056 ) ) ;
#8644 = CIRCLE ( 'NONE', #154, 2.000000000000000000 ) ;
#8645 = CARTESIAN_POINT ( 'NONE',  ( -2.303009741871944172E-17, 0.8232575913728890082, -1.453755053663958216E-18 ) ) ;
#8646 = DIRECTION ( 'NONE',  ( 0.000000000000000000, 0.000000000000000000, 1.000000000000000000 ) ) ;
#8647 = VERTEX_POINT ( 'NONE', #10240 ) ;
#8648 = CARTESIAN_POINT ( 'NONE',  ( -49.99999999999999289, 120.0000000000000142, 0.5000000000000000000 ) ) ;
#8649 = FACE_OUTER_BOUND ( 'NONE', #1570, .T. ) ;
#8650 = ORIENTED_EDGE ( 'NONE', *, *, #8901, .T. ) ;
#8651 = CARTESIAN_POINT ( 'NONE',  ( 58.70736094381068426, -9.392073098158828515, -8.673617379884035472E-16 ) ) ;
#8652 = VERTEX_POINT ( 'NONE', #12277 ) ;
#8653 = DIRECTION ( 'NONE',  ( 1.000000000000000000, 0.000000000000000000, 0.000000000000000000 ) ) ;
#8654 = CARTESIAN_POINT ( 'NONE',  ( -15.29705854078138927, 55.48535772202409788, -30.59411708156277854 ) ) ;
#8655 = CARTESIAN_POINT ( 'NONE',  ( 34.25812584745457912, 108.1980041606221334, -0.6234749816336034867 ) ) ;
#8656 = CARTESIAN_POINT ( 'NONE',  ( 10.69381717166375623, 25.55944687211528077, 1.274859266482038215E-15 ) ) ;
#8657 = CARTESIAN_POINT ( 'NONE',  ( 40.81228451836345528, 100.6358150620708329, 0.5000000000000000000 ) ) ;
#8658 = CARTESIAN_POINT ( 'NONE',  ( -18.54049621773915746, 27.07720798311999388, -7.500000000000000000 ) ) ;
#8659 = ADVANCED_FACE ( 'NONE', ( #3560 ), #6934, .T. ) ;
#8660 = LINE ( 'NONE', #1102, #2429 ) ;
#8661 = ADVANCED_FACE ( 'NONE', ( #5746 ), #1277, .T. ) ;
#8662 = CYLINDRICAL_SURFACE ( 'NONE', #13006, 40.00000000000001421 ) ;
#8663 = AXIS2_PLACEMENT_3D ( 'NONE', #4875, #2634, #9091 ) ;
#8664 = ORIENTED_EDGE ( 'NONE', *, *, #3610, .T. ) ;
#8665 = ADVANCED_FACE ( 'NONE', ( #1687 ), #2809, .T. ) ;
#8666 = EDGE_CURVE ( 'NONE', #5463, #9616, #7136, .T. ) ;
#8667 = ORIENTED_EDGE ( 'NONE', *, *, #12038, .T. ) ;
#8668 = DIRECTION ( 'NONE',  ( 1.000000000000000000, 0.000000000000000000, 0.000000000000000000 ) ) ;
#8669 = ORIENTED_EDGE ( 'NONE', *, *, #7900, .T. ) ;
#8670 = CARTESIAN_POINT ( 'NONE',  ( 18.71826692230518674, -9.296782722394514309, -2.500000000000002665 ) ) ;
#8671 = CARTESIAN_POINT ( 'NONE',  ( -25.00000000000000355, 120.0000000000000142, -2.499999999999998668 ) ) ;
#8672 = DIRECTION ( 'NONE',  ( 1.086108692045681373E-16, -1.448144922727572616E-16, 1.000000000000000000 ) ) ;
#8673 = EDGE_CURVE ( 'NONE', #2108, #3901, #13443, .T. ) ;
#8674 = CARTESIAN_POINT ( 'NONE',  ( 15.29705854078138216, 10.24803554138234318, 30.59411708156277498 ) ) ;
#8675 = ORIENTED_EDGE ( 'NONE', *, *, #11665, .T. ) ;
#8676 = VERTEX_POINT ( 'NONE', #12566 ) ;
#8677 = EDGE_CURVE ( 'NONE', #4998, #3518, #12962, .T. ) ;
#8678 = EDGE_CURVE ( 'NONE', #10096, #1833, #650, .T. ) ;
#8679 = ORIENTED_EDGE ( 'NONE', *, *, #7285, .T. ) ;
#8680 = DIRECTION ( 'NONE',  ( -1.000000000000000000, 0.000000000000000000, 0.000000000000000000 ) ) ;
#8681 = ORIENTED_EDGE ( 'NONE', *, *, #6212, .F. ) ;
#8682 = CARTESIAN_POINT ( 'NONE',  ( -2.237684797877294057E-15, 79.99058638175036151, -1.412519245696701404E-16 ) ) ;
#8683 = AXIS2_PLACEMENT_3D ( 'NONE', #7869, #6054, #596 ) ;
#8684 = FACE_OUTER_BOUND ( 'NONE', #10749, .T. ) ;
#8685 = VECTOR ( 'NONE', #9046, 1000.000000000000000 ) ;
#8686 = CARTESIAN_POINT ( 'NONE',  ( 40.81228451836345528, 100.6358150620708329, -0.5000000000000000000 ) ) ;
#8687 = CARTESIAN_POINT ( 'NONE',  ( 3.828023344975119535, 90.45717703472961091, -3.219997411495246098 ) ) ;
#8688 = CARTESIAN_POINT ( 'NONE',  ( 0.9252956712946845963, -80.77513221109299479, 9.969903607383971078 ) ) ;
#8689 = DIRECTION ( 'NONE',  ( -0.000000000000000000, 0.000000000000000000, -1.000000000000000000 ) ) ;
#8690 = ORIENTED_EDGE ( 'NONE', *, *, #13865, .F. ) ;
#8691 = ORIENTED_EDGE ( 'NONE', *, *, #4212, .F. ) ;
#8692 = ORIENTED_EDGE ( 'NONE', *, *, #6118, .T. ) ;
#8693 = AXIS2_PLACEMENT_3D ( 'NONE', #4242, #3196, #7474 ) ;
#8694 = DIRECTION ( 'NONE',  ( 1.000000000000000000, 0.000000000000000000, -0.000000000000000000 ) ) ;
#8695 = ORIENTED_EDGE ( 'NONE', *, *, #13218, .F. ) ;
#8696 = CARTESIAN_POINT ( 'NONE',  ( 25.00000000000001421, -34.99999999999999289, 7.500000000000000000 ) ) ;
#8697 = SURFACE_STYLE_FILL_AREA ( #7576 ) ;
#8698 = DIRECTION ( 'NONE',  ( -0.000000000000000000, -0.000000000000000000, 1.000000000000000000 ) ) ;
#8699 = LINE ( 'NONE', #3369, #671 ) ;
#8700 = FACE_OUTER_BOUND ( 'NONE', #4913, .T. ) ;
#8701 = DIRECTION ( 'NONE',  ( 0.000000000000000000, 0.000000000000000000, -1.000000000000000000 ) ) ;
#8702 = CARTESIAN_POINT ( 'NONE',  ( -9.841115069317030617, -69.87878787878872799, -2.624300023644856150 ) ) ;
#8703 = AXIS2_PLACEMENT_3D ( 'NONE', #1915, #6204, #10465 ) ;
#8704 = FACE_OUTER_BOUND ( 'NONE', #13205, .T. ) ;
#8705 = LINE ( 'NONE', #11867, #13091 ) ;
#8706 = ORIENTED_EDGE ( 'NONE', *, *, #13764, .F. ) ;
#8707 = CARTESIAN_POINT ( 'NONE',  ( -35.00000000000000000, -4.286263797015736496E-15, -4.000000000000000000 ) ) ;
#8708 = VERTEX_POINT ( 'NONE', #12696 ) ;
#8709 = CARTESIAN_POINT ( 'NONE',  ( 60.47785218637952198, 1.062566689801825781, 2.168404344971008868E-15 ) ) ;
#8710 = CARTESIAN_POINT ( 'NONE',  ( -24.99999999999998934, -100.0000000000065938, -5.046127144261280506 ) ) ;
#8711 = CIRCLE ( 'NONE', #2685, 4.999999999999997335 ) ;
#8712 = DIRECTION ( 'NONE',  ( -0.8000000000000008216, -0.5999999999999988676, -0.000000000000000000 ) ) ;
#8713 = VERTEX_POINT ( 'NONE', #13776 ) ;
#8714 = CARTESIAN_POINT ( 'NONE',  ( 14.79219767565756527, 6.218900627562690353, 2.500000000000000444 ) ) ;
#8715 = DIRECTION ( 'NONE',  ( 0.000000000000000000, 0.000000000000000000, 1.000000000000000000 ) ) ;
#8716 = AXIS2_PLACEMENT_3D ( 'NONE', #7253, #751, #13618 ) ;
#8717 = DIRECTION ( 'NONE',  ( 0.000000000000000000, 0.000000000000000000, -1.000000000000000000 ) ) ;
#8718 = CARTESIAN_POINT ( 'NONE',  ( 34.28525802518650778, 108.1064455385057812, -1.101804919165826124 ) ) ;
#8719 = CARTESIAN_POINT ( 'NONE',  ( 36.50000000000000711, 113.0000000000000142, -7.500000000000000000 ) ) ;
#8720 = CARTESIAN_POINT ( 'NONE',  ( 48.99302833075611119, 12.47878836808089886, 2.500000000000004441 ) ) ;
#8721 = CARTESIAN_POINT ( 'NONE',  ( 40.68412312724077395, 100.6732077982500897, 1.167148848990505750 ) ) ;
#8722 = DIRECTION ( 'NONE',  ( 0.000000000000000000, 0.000000000000000000, 1.000000000000000000 ) ) ;
#8723 = AXIS2_PLACEMENT_3D ( 'NONE', #5499, #1359, #7669 ) ;
#8724 = AXIS2_PLACEMENT_3D ( 'NONE', #8774, #12872, #13086 ) ;
#8725 = DIRECTION ( 'NONE',  ( -0.000000000000000000, -0.000000000000000000, -1.000000000000000000 ) ) ;
#8726 = AXIS2_PLACEMENT_3D ( 'NONE', #8645, #7658, #9701 ) ;
#8727 = DIRECTION ( 'NONE',  ( 1.000000000000000000, 0.000000000000000000, 0.000000000000000000 ) ) ;
#8728 = AXIS2_PLACEMENT_3D ( 'NONE', #13783, #2096, #12575 ) ;
#8729 = ORIENTED_EDGE ( 'NONE', *, *, #11995, .F. ) ;
#8730 = LINE ( 'NONE', #4596, #9207 ) ;
#8731 = ORIENTED_EDGE ( 'NONE', *, *, #10531, .F. ) ;
#8732 = CARTESIAN_POINT ( 'NONE',  ( -22.00000000000000000, -35.00000000000000000, -7.500000000000000000 ) ) ;
#8733 = EDGE_CURVE ( 'NONE', #11307, #11449, #7558, .T. ) ;
#8734 = B_SPLINE_CURVE_WITH_KNOTS ( 'NONE', 3,
 ( #8657, #1173, #6693, #1366, #8721, #11814, #5428, #7601, #2205, #2280, #8795, #3461, #6492, #11885, #4589, #10820 ),
 .UNSPECIFIED., .F., .F.,
 ( 4, 2, 2, 2, 2, 2, 2, 4 ),
 ( 1.967444805628318194E-07, 0.0004077652619395025148, 0.0008153337793984422781, 0.001630470814316321588, 0.002038039331775261514, 0.002445607849234201006, 0.002853176366693140498, 0.003260744884152080424 ),
 .UNSPECIFIED. ) ;
#8735 = CIRCLE ( 'NONE', #9865, 4.999999999999998224 ) ;
#8736 = EDGE_CURVE ( 'NONE', #2229, #4279, #13843, .T. ) ;
#8737 = EDGE_LOOP ( 'NONE', ( #3197, #1220, #440, #8913, #2995 ) ) ;
#8738 = CARTESIAN_POINT ( 'NONE',  ( -2.866821506922881722E-16, 10.24803554138234496, -1.809656371776380929E-17 ) ) ;
#8739 = CIRCLE ( 'NONE', #6720, 2.500000000000002220 ) ;
#8740 = AXIS2_PLACEMENT_3D ( 'NONE', #2332, #8785, #1225 ) ;
#8741 = LINE ( 'NONE', #13044, #1946 ) ;
#8742 = EDGE_CURVE ( 'NONE', #6892, #4054, #13572, .T. ) ;
#8743 = EDGE_CURVE ( 'NONE', #7988, #13719, #10576, .T. ) ;
#8744 = DIRECTION ( 'NONE',  ( -2.797435172181481150E-17, 1.000000000000000000, -1.765856845898762549E-18 ) ) ;
#8745 = ORIENTED_EDGE ( 'NONE', *, *, #3442, .F. ) ;
#8746 = ORIENTED_EDGE ( 'NONE', *, *, #5929, .F. ) ;
#8747 = AXIS2_PLACEMENT_3D ( 'NONE', #6310, #9193, #10839 ) ;
#8748 = EDGE_CURVE ( 'NONE', #8021, #6030, #10312, .T. ) ;
#8749 = CARTESIAN_POINT ( 'NONE',  ( 8.385254915620288685, 53.02855864072483882, 9.355740606675293587E-16 ) ) ;
#8750 = EDGE_CURVE ( 'NONE', #1592, #3741, #6670, .T. ) ;
#8751 = EDGE_LOOP ( 'NONE', ( #589, #12539, #1590, #4229 ) ) ;
#8752 = CARTESIAN_POINT ( 'NONE',  ( 31.01425004688410070, -18.32044754671509423, -2.500000000000004441 ) ) ;
#8753 = DIRECTION ( 'NONE',  ( 0.000000000000000000, 0.000000000000000000, -1.000000000000000000 ) ) ;
#8754 = CARTESIAN_POINT ( 'NONE',  ( 41.99999999999999289, 120.0000000000000284, -0.5000000000000000000 ) ) ;
#8755 = EDGE_CURVE ( 'NONE', #10021, #6151, #9810, .T. ) ;
#8756 = AXIS2_PLACEMENT_3D ( 'NONE', #10270, #3750, #11384 ) ;
#8757 = CARTESIAN_POINT ( 'NONE',  ( -24.99999999999998934, -99.15310334213020838, 4.530792947966844994E-20 ) ) ;
#8758 = CARTESIAN_POINT ( 'NONE',  ( -40.81228451836347659, 100.6358150620708471, 0.5000000000000000000 ) ) ;
#8759 = CARTESIAN_POINT ( 'NONE',  ( -3.408847948936934547, -84.09052683291464803, 8.956775459301910658 ) ) ;
#8760 = CARTESIAN_POINT ( 'NONE',  ( 15.29705854078139105, 27.21102387199583816, 1.823632900916640874E-15 ) ) ;
#8761 = ORIENTED_EDGE ( 'NONE', *, *, #7894, .F. ) ;
#8762 = VERTEX_POINT ( 'NONE', #2948 ) ;
#8763 = ORIENTED_EDGE ( 'NONE', *, *, #7360, .T. ) ;
#8764 = AXIS2_PLACEMENT_3D ( 'NONE', #13302, #2752, #6745 ) ;
#8765 = DIRECTION ( 'NONE',  ( 0.000000000000000000, 0.000000000000000000, 1.000000000000000000 ) ) ;
#8766 = CARTESIAN_POINT ( 'NONE',  ( -34.99999999999999289, -97.00000000000000000, -7.500000000000000000 ) ) ;
#8767 = ORIENTED_EDGE ( 'NONE', *, *, #6103, .F. ) ;
#8768 = LINE ( 'NONE', #11009, #4097 ) ;
#8769 = DIRECTION ( 'NONE',  ( 0.9960067511297464593, -0.08927794634716622324, 3.401418580343279473E-17 ) ) ;
#8770 = CARTESIAN_POINT ( 'NONE',  ( 15.29705854078138749, 57.37192529142945574, 1.773704474924340737E-15 ) ) ;
#8771 = LINE ( 'NONE', #6401, #9170 ) ;
#8772 = CARTESIAN_POINT ( 'NONE',  ( 1.956031471770903973, -154.2164502167725857, 1.283490743971270831 ) ) ;
#8773 = CYLINDRICAL_SURFACE ( 'NONE', #10055, 27.49999999999999289 ) ;
#8774 = CARTESIAN_POINT ( 'NONE',  ( -35.00000000000000000, -4.286263797015736496E-15, 10.49999999999999822 ) ) ;
#8775 = EDGE_CURVE ( 'NONE', #12409, #11721, #1301, .T. ) ;
#8776 = CARTESIAN_POINT ( 'NONE',  ( -0.9402774206043360561, -80.12121212121206781, -9.996606859377621390 ) ) ;
#8777 = FACE_OUTER_BOUND ( 'NONE', #4769, .T. ) ;
#8778 = CYLINDRICAL_SURFACE ( 'NONE', #9713, 69.99999999999998579 ) ;
#8779 = ORIENTED_EDGE ( 'NONE', *, *, #8953, .T. ) ;
#8780 = FACE_OUTER_BOUND ( 'NONE', #10721, .T. ) ;
#8781 = CARTESIAN_POINT ( 'NONE',  ( 8.385254915620288685, 71.87811454074363837, -16.77050983124057382 ) ) ;
#8782 = ORIENTED_EDGE ( 'NONE', *, *, #11673, .T. ) ;
#8783 = VECTOR ( 'NONE', #2201, 1000.000000000000000 ) ;
#8784 = FACE_OUTER_BOUND ( 'NONE', #1605, .T. ) ;
#8785 = DIRECTION ( 'NONE',  ( -2.797435172181481150E-17, 1.000000000000000000, -1.765856845898762549E-18 ) ) ;
#8786 = ORIENTED_EDGE ( 'NONE', *, *, #9317, .T. ) ;
#8787 = AXIS2_PLACEMENT_3D ( 'NONE', #9926, #10069, #4746 ) ;
#8788 = DIRECTION ( 'NONE',  ( 1.000000000000000000, 2.797435172181480534E-17, 0.000000000000000000 ) ) ;
#8789 = ORIENTED_EDGE ( 'NONE', *, *, #6178, .T. ) ;
#8790 = DIRECTION ( 'NONE',  ( -2.797435172181481150E-17, 1.000000000000000000, -1.765856845898762549E-18 ) ) ;
#8791 = CARTESIAN_POINT ( 'NONE',  ( -15.29705854078139637, 0.8232575913729158756, -1.876256887941090008E-15 ) ) ;
#8792 = DIRECTION ( 'NONE',  ( 1.000000000000000000, 0.000000000000000000, 0.000000000000000000 ) ) ;
#8793 = CARTESIAN_POINT ( 'NONE',  ( -8.385254915620292238, -3.520109059331727686, 6.216008680731233110E-18 ) ) ;
#8794 = CARTESIAN_POINT ( 'NONE',  ( 18.54049621773915746, 27.07720798312000809, -7.500000000000000000 ) ) ;
#8795 = CARTESIAN_POINT ( 'NONE',  ( 39.64259366921353944, 101.1295926276828538, 2.298140577494254266 ) ) ;
#8796 = CARTESIAN_POINT ( 'NONE',  ( 26.79177319725820539, -26.24642857144861807, 4.000000000000000000 ) ) ;
#8797 = AXIS2_PLACEMENT_3D ( 'NONE', #12407, #10160, #8968 ) ;
#8798 = CARTESIAN_POINT ( 'NONE',  ( 82.09155748149851206, -71.43674177705591433, 2.500000000000000000 ) ) ;
#8799 = EDGE_CURVE ( 'NONE', #12162, #6130, #3098, .T. ) ;
#8800 = ORIENTED_EDGE ( 'NONE', *, *, #3955, .T. ) ;
#8801 = DIRECTION ( 'NONE',  ( 0.000000000000000000, 0.000000000000000000, -1.000000000000000000 ) ) ;
#8802 = ORIENTED_EDGE ( 'NONE', *, *, #3548, .T. ) ;
#8803 = CIRCLE ( 'NONE', #2780, 25.50000000002549783 ) ;
#8804 = CARTESIAN_POINT ( 'NONE',  ( -52.50000000000000000, 120.0000000000000142, 7.500000000000000000 ) ) ;
#8805 = SHAPE_DEFINITION_REPRESENTATION ( #10664, #2342 ) ;
#8806 = ORIENTED_EDGE ( 'NONE', *, *, #1291, .F. ) ;
#8807 = DIRECTION ( 'NONE',  ( 1.000000000000000000, 0.000000000000000000, 0.000000000000000000 ) ) ;
#8808 = CARTESIAN_POINT ( 'NONE',  ( 8.385254915620290461, 53.02855864072483882, 2.053795118489800004E-15 ) ) ;
#8809 = DIRECTION ( 'NONE',  ( 1.000000000000000000, 0.000000000000000000, 0.000000000000000000 ) ) ;
#8810 = CARTESIAN_POINT ( 'NONE',  ( 34.99999999999958789, 1.104930248025249758E-13, -2.499999999999999112 ) ) ;
#8811 = AXIS2_PLACEMENT_3D ( 'NONE', #11338, #9100, #7976 ) ;
#8812 = ADVANCED_FACE ( 'NONE', ( #8469 ), #6038, .T. ) ;
#8813 = ORIENTED_EDGE ( 'NONE', *, *, #4117, .F. ) ;
#8814 = ADVANCED_FACE ( 'NONE', ( #13643 ), #3990, .T. ) ;
#8815 = CARTESIAN_POINT ( 'NONE',  ( 15.29705854078138927, 29.09759144140119957, 1.823632900916640086E-15 ) ) ;
#8816 = EDGE_CURVE ( 'NONE', #3113, #3156, #1979, .T. ) ;
#8817 = ORIENTED_EDGE ( 'NONE', *, *, #4700, .T. ) ;
#8818 = ORIENTED_EDGE ( 'NONE', *, *, #13603, .T. ) ;
#8819 = CARTESIAN_POINT ( 'NONE',  ( 8.385254915620281579, 71.87811454074363837, 16.77050983124057737 ) ) ;
#8820 = AXIS2_PLACEMENT_3D ( 'NONE', #9448, #13693, #7465 ) ;
#8821 = CARTESIAN_POINT ( 'NONE',  ( 9.857979974958242408, 4.257796268226277547, 2.499999999999999556 ) ) ;
#8822 = SURFACE_STYLE_USAGE ( .BOTH. , #4544 ) ;
#8823 = CARTESIAN_POINT ( 'NONE',  ( 8.385254915620292238, -12.94488700934118341, 1.052073721316228694E-15 ) ) ;
#8824 = DIRECTION ( 'NONE',  ( 1.000000000000000000, 0.000000000000000000, 0.000000000000000000 ) ) ;
#8825 = CARTESIAN_POINT ( 'NONE',  ( -0.9919461901367589984, -82.18142821831455080, 9.724687322501905484 ) ) ;
#8826 = DIRECTION ( 'NONE',  ( -0.000000000000000000, -0.000000000000000000, -1.000000000000000000 ) ) ;
#8827 = ORIENTED_EDGE ( 'NONE', *, *, #10894, .F. ) ;
#8828 = EDGE_CURVE ( 'NONE', #12409, #8361, #7686, .T. ) ;
#8829 = ORIENTED_EDGE ( 'NONE', *, *, #6549, .T. ) ;
#8830 = ADVANCED_FACE ( 'NONE', ( #1053, #5517 ), #11830, .T. ) ;
#8831 = ORIENTED_EDGE ( 'NONE', *, *, #133, .T. ) ;
#8832 = CIRCLE ( 'NONE', #5467, 2.000000000000003997 ) ;
#8833 = EDGE_CURVE ( 'NONE', #1472, #7475, #6027, .T. ) ;
#8834 = EDGE_CURVE ( 'NONE', #8676, #5851, #1756, .T. ) ;
#8835 = CARTESIAN_POINT ( 'NONE',  ( -4.230699918504780221, 91.18539124371005755, 2.666380740812165584 ) ) ;
#8836 = DIRECTION ( 'NONE',  ( -6.158143864569485777E-17, -2.736152283717910599E-16, 1.000000000000000000 ) ) ;
#8837 = ORIENTED_EDGE ( 'NONE', *, *, #9875, .F. ) ;
#8838 = CARTESIAN_POINT ( 'NONE',  ( 26.09988479906369463, 19.17858047941126642, -2.499999999999993783 ) ) ;
#8839 = CARTESIAN_POINT ( 'NONE',  ( -8.385254915620292238, 34.17900274070598243, -1.147608011196236061E-15 ) ) ;
#8840 = CARTESIAN_POINT ( 'NONE',  ( -6.190615655759536180E-16, 22.12961257269105531, -3.907772785857374249E-17 ) ) ;
#8841 = CARTESIAN_POINT ( 'NONE',  ( -0.2890385494233511099, -128.7272727272755048, 4.499839249777335404 ) ) ;
#8842 = CARTESIAN_POINT ( 'NONE',  ( -2.079471018873752021E-15, 74.33491362204294717, -1.312648161087776599E-16 ) ) ;
#8843 = CARTESIAN_POINT ( 'NONE',  ( 12.99553232110414669, -17.19957910547634228, 1.630511914918685592E-15 ) ) ;
#8844 = AXIS2_PLACEMENT_3D ( 'NONE', #3114, #11740, #10421 ) ;
#8845 = DIRECTION ( 'NONE',  ( -2.797435172181481150E-17, 1.000000000000000000, -1.765856845898762549E-18 ) ) ;
#8846 = DIRECTION ( 'NONE',  ( -1.000000000000000000, 0.000000000000000000, 0.000000000000000000 ) ) ;
#8847 = DIRECTION ( 'NONE',  ( 0.000000000000000000, 0.000000000000000000, -1.000000000000000000 ) ) ;
#8848 = CIRCLE ( 'NONE', #9088, 5.000000000000000000 ) ;
#8849 = CARTESIAN_POINT ( 'NONE',  ( 0.000000000000000000, 40.00000000000000000, 0.000000000000000000 ) ) ;
#8850 = AXIS2_PLACEMENT_3D ( 'NONE', #8219, #10594, #7163 ) ;
#8851 = ADVANCED_FACE ( 'NONE', ( #4528 ), #5575, .T. ) ;
#8852 = ORIENTED_EDGE ( 'NONE', *, *, #12471, .T. ) ;
#8853 = ORIENTED_EDGE ( 'NONE', *, *, #8510, .T. ) ;
#8854 = DIRECTION ( 'NONE',  ( -0.000000000000000000, -0.000000000000000000, -1.000000000000000000 ) ) ;
#8855 = CARTESIAN_POINT ( 'NONE',  ( 37.50000000000000711, 4.592425496802575156E-15, 4.000000000000000000 ) ) ;
#8856 = VECTOR ( 'NONE', #6063, 1000.000000000000000 ) ;
#8857 = EDGE_CURVE ( 'NONE', #3876, #2956, #3534, .T. ) ;
#8858 = CARTESIAN_POINT ( 'NONE',  ( 34.99999999999958789, 1.104930248025249758E-13, -2.499999999999999112 ) ) ;
#8859 = CARTESIAN_POINT ( 'NONE',  ( 34.99999999999958789, 1.091249486606660213E-13, 2.500000000000000000 ) ) ;
#8860 = CARTESIAN_POINT ( 'NONE',  ( -60.00000000000001421, -4.286263797015736496E-15, 7.500000000000000000 ) ) ;
#8861 = ORIENTED_EDGE ( 'NONE', *, *, #5868, .F. ) ;
#8862 = ORIENTED_EDGE ( 'NONE', *, *, #5229, .F. ) ;
#8863 = CARTESIAN_POINT ( 'NONE',  ( 8.385254915620294014, -15.56949922734665570, 1.052073721316228694E-15 ) ) ;
#8864 = ORIENTED_EDGE ( 'NONE', *, *, #9547, .F. ) ;
#8865 = AXIS2_PLACEMENT_3D ( 'NONE', #8170, #8307, #748 ) ;
#8866 = DIRECTION ( 'NONE',  ( 1.000000000000000000, 0.000000000000000000, 0.000000000000000000 ) ) ;
#8867 = CARTESIAN_POINT ( 'NONE',  ( 8.385254915620294014, 24.75422479069652582, 2.053795118489800793E-15 ) ) ;
#8868 = DIRECTION ( 'NONE',  ( -0.000000000000000000, -0.000000000000000000, -1.000000000000000000 ) ) ;
#8869 = ADVANCED_FACE ( 'NONE', ( #6371 ), #8539, .T. ) ;
#8870 = CARTESIAN_POINT ( 'NONE',  ( 34.46489652880494248, 107.6161854625081276, -1.920135329999817175 ) ) ;
#8871 = FACE_BOUND ( 'NONE', #8213, .T. ) ;
#8872 = CARTESIAN_POINT ( 'NONE',  ( -9.943536534200680066, -71.42980831791368246, -1.832023084373848532 ) ) ;
#8873 = DIRECTION ( 'NONE',  ( -1.000000000000000000, 0.000000000000000000, 0.000000000000000000 ) ) ;
#8874 = CIRCLE ( 'NONE', #11339, 15.29705854078139282 ) ;
#8875 = DIRECTION ( 'NONE',  ( -2.797435172181481150E-17, 1.000000000000000000, -1.765856845898762549E-18 ) ) ;
#8876 = CARTESIAN_POINT ( 'NONE',  ( -10.69381717166375623, 16.13466892210585613, -1.366597928139322991E-15 ) ) ;
#8877 = ORIENTED_EDGE ( 'NONE', *, *, #1891, .F. ) ;
#8878 = DIRECTION ( 'NONE',  ( -0.000000000000000000, -0.000000000000000000, -1.000000000000000000 ) ) ;
#8879 = EDGE_LOOP ( 'NONE', ( #4825, #7392, #8023, #12106 ) ) ;
#8880 = DIRECTION ( 'NONE',  ( -1.000000000000000000, 0.000000000000000000, 0.000000000000000000 ) ) ;
#8881 = AXIS2_PLACEMENT_3D ( 'NONE', #4253, #8603, #11897 ) ;
#8882 = B_SPLINE_CURVE_WITH_KNOTS ( 'NONE', 3,
 ( #150, #12046, #12982, #8749 ),
 .UNSPECIFIED., .F., .F.,
 ( 4, 4 ),
 ( 0.000000000000000000, 1.000000000000000000 ),
 .UNSPECIFIED. ) ;
#8883 = ORIENTED_EDGE ( 'NONE', *, *, #5674, .T. ) ;
#8884 = CARTESIAN_POINT ( 'NONE',  ( -26.79177319725820894, -26.24642857144861807, -4.000000000000000000 ) ) ;
#8885 = ORIENTED_EDGE ( 'NONE', *, *, #11581, .F. ) ;
#8886 = CARTESIAN_POINT ( 'NONE',  ( -35.00000000000000711, -25.00000000000000711, 7.500000000000000000 ) ) ;
#8887 = CARTESIAN_POINT ( 'NONE',  ( -39.64464840659820766, 101.1283747906781088, 2.297097423097428592 ) ) ;
#8888 = CYLINDRICAL_SURFACE ( 'NONE', #10581, 25.50000000002550138 ) ;
#8889 = CARTESIAN_POINT ( 'NONE',  ( 37.49999999999999289, 120.0000000000000142, 2.499999999999999556 ) ) ;
#8890 = VERTEX_POINT ( 'NONE', #5585 ) ;
#8891 = PRODUCT_DEFINITION_SHAPE ( 'NONE', 'NONE',  #13905 ) ;
#8892 = APPLICATION_CONTEXT ( 'automotive_design' ) ;
#8893 = CARTESIAN_POINT ( 'NONE',  ( 16.34455450841069890, -1.870656171256065425, -2.500000000000000888 ) ) ;
#8894 = VERTEX_POINT ( 'NONE', #9732 ) ;
#8895 = LINE ( 'NONE', #1530, #4728 ) ;
#8896 = ORIENTED_EDGE ( 'NONE', *, *, #11057, .T. ) ;
#8897 = ORIENTED_EDGE ( 'NONE', *, *, #12026, .F. ) ;
#8898 = DIRECTION ( 'NONE',  ( -1.000000000000000000, 0.000000000000000000, 0.000000000000000000 ) ) ;
#8899 = VERTEX_POINT ( 'NONE', #11696 ) ;
#8900 = CARTESIAN_POINT ( 'NONE',  ( 1.653273178848927024E-14, -135.0000000000000000, 0.000000000000000000 ) ) ;
#8901 = EDGE_CURVE ( 'NONE', #8113, #4900, #2089, .T. ) ;
#8902 = DIRECTION ( 'NONE',  ( -1.000000000000000000, 0.000000000000000000, 0.000000000000000000 ) ) ;
#8903 = CARTESIAN_POINT ( 'NONE',  ( 18.78199004159288066, 27.01526789321293265, 6.903011289631059810 ) ) ;
#8904 = DIRECTION ( 'NONE',  ( -1.000000000000000000, 0.000000000000000000, 0.000000000000000000 ) ) ;
#8905 = DIRECTION ( 'NONE',  ( -6.158143864569485777E-17, -2.736152283717910599E-16, 1.000000000000000000 ) ) ;
#8906 = CARTESIAN_POINT ( 'NONE',  ( -8.385254915620295790, 59.82872437272870769, 16.77050983124058092 ) ) ;
#8907 = PRODUCT_RELATED_PRODUCT_CATEGORY ( 'part', '', ( #13292 ) ) ;
#8908 = ORIENTED_EDGE ( 'NONE', *, *, #1538, .T. ) ;
#8909 = AXIS2_PLACEMENT_3D ( 'NONE', #3134, #907, #1953 ) ;
#8910 = ORIENTED_EDGE ( 'NONE', *, *, #12889, .F. ) ;
#8911 = ORIENTED_EDGE ( 'NONE', *, *, #17, .T. ) ;
#8912 = CARTESIAN_POINT ( 'NONE',  ( -10.00000000000000000, 99.99999999999994316, 0.5000000000000000000 ) ) ;
#8913 = ORIENTED_EDGE ( 'NONE', *, *, #4759, .F. ) ;
#8914 = CARTESIAN_POINT ( 'NONE',  ( 8.385254915620292238, -24.99427717735608567, 16.77050983124059158 ) ) ;
#8915 = DIRECTION ( 'NONE',  ( -2.797435172181481150E-17, 1.000000000000000000, -1.765856845898762549E-18 ) ) ;
#8916 = EDGE_LOOP ( 'NONE', ( #8430, #12572, #13059, #5439 ) ) ;
#8917 = CARTESIAN_POINT ( 'NONE',  ( 1.087924128445332483, -78.56626503148619634, 10.04922990102044622 ) ) ;
#8918 = AXIS2_PLACEMENT_3D ( 'NONE', #8353, #992, #5257 ) ;
#8919 = CARTESIAN_POINT ( 'NONE',  ( -12.99553232110413425, 58.19864449459908684, -25.99106464220827561 ) ) ;
#8920 = ADVANCED_FACE ( 'NONE', ( #5376 ), #3343, .T. ) ;
#8921 = CYLINDRICAL_SURFACE ( 'NONE', #781, 12.49999999999999289 ) ;
#8922 = LINE ( 'NONE', #2464, #12527 ) ;
#8923 = DIRECTION ( 'NONE',  ( -2.797435172181481150E-17, 1.000000000000000000, -1.765856845898762549E-18 ) ) ;
#8924 = CARTESIAN_POINT ( 'NONE',  ( -2.264596963716165146, -106.9090909090919013, 6.916633125701347140 ) ) ;
#8925 = ADVANCED_FACE ( 'NONE', ( #12841 ), #7485, .T. ) ;
#8926 = DIRECTION ( 'NONE',  ( -6.158143864569485777E-17, -2.736152283717910599E-16, 1.000000000000000000 ) ) ;
#8927 = CARTESIAN_POINT ( 'NONE',  ( 35.06230589874905945, 106.5835921350012683, 2.499999999999999556 ) ) ;
#8928 = EDGE_CURVE ( 'NONE', #9797, #2621, #4325, .T. ) ;
#8929 = FACE_OUTER_BOUND ( 'NONE', #3538, .T. ) ;
#8930 = EDGE_CURVE ( 'NONE', #11500, #4518, #6912, .T. ) ;
#8931 = VERTEX_POINT ( 'NONE', #6571 ) ;
#8932 = ORIENTED_EDGE ( 'NONE', *, *, #11387, .F. ) ;
#8933 = VECTOR ( 'NONE', #6177, 1000.000000000000000 ) ;
#8934 = DIRECTION ( 'NONE',  ( 0.000000000000000000, 0.000000000000000000, 1.000000000000000000 ) ) ;
#8935 = VERTEX_POINT ( 'NONE', #13198 ) ;
#8936 = CIRCLE ( 'NONE', #4674, 9.000000000008999024 ) ;
#8937 = DIRECTION ( 'NONE',  ( 1.000000000000000000, 0.000000000000000000, 0.000000000000000000 ) ) ;
#8938 = DIRECTION ( 'NONE',  ( -0.000000000000000000, 1.000000000000000000, 0.000000000000000000 ) ) ;
#8939 = DIRECTION ( 'NONE',  ( 0.9960067511297463483, -0.08927794634716620936, 4.626175998653454121E-17 ) ) ;
#8940 = DIRECTION ( 'NONE',  ( 0.7533101279583153120, -0.6576654553155629745, -1.387852799596036359E-16 ) ) ;
#8941 = LINE ( 'NONE', #5421, #2933 ) ;
#8942 = EDGE_LOOP ( 'NONE', ( #7550, #8477, #3859 ) ) ;
#8943 = CARTESIAN_POINT ( 'NONE',  ( 10.69346802281034847, -16.37459952631584059, 0.000000000000000000 ) ) ;
#8944 = ORIENTED_EDGE ( 'NONE', *, *, #6118, .F. ) ;
#8945 = LINE ( 'NONE', #5496, #9071 ) ;
#8946 = AXIS2_PLACEMENT_3D ( 'NONE', #3277, #11899, #2291 ) ;
#8947 = DIRECTION ( 'NONE',  ( 0.000000000000000000, 0.000000000000000000, 1.000000000000000000 ) ) ;
#8948 = CARTESIAN_POINT ( 'NONE',  ( -35.00000000000000000, -35.00000000000000000, 7.500000000000000000 ) ) ;
#8949 = CARTESIAN_POINT ( 'NONE',  ( -25.00000000000000355, 120.0000000000000142, 2.499999999999999556 ) ) ;
#8950 = DIRECTION ( 'NONE',  ( 0.01532218268401990685, -0.9998826084685129567, -2.775705599192072226E-16 ) ) ;
#8951 = CARTESIAN_POINT ( 'NONE',  ( -4.789632183893028028, -77.94522261687450282, -8.921723405160534526 ) ) ;
#8952 = CARTESIAN_POINT ( 'NONE',  ( 34.66997162884352690, 21.14050806081579736, -2.499999999999992895 ) ) ;
#8953 = EDGE_CURVE ( 'NONE', #13310, #12007, #2895, .T. ) ;
#8954 = CARTESIAN_POINT ( 'NONE',  ( -15.29705854078138749, -36.87585420866476227, 6.511747960273540061E-17 ) ) ;
#8955 = CARTESIAN_POINT ( 'NONE',  ( -10.69381717166375800, 16.13466892210585257, 21.38763434332750890 ) ) ;
#8956 = DIRECTION ( 'NONE',  ( -1.000000000000000000, 0.000000000000000000, 0.000000000000000000 ) ) ;
#8957 = CARTESIAN_POINT ( 'NONE',  ( 3.632360187558549836, 90.29910261214918421, 3.439149220787172556 ) ) ;
#8958 = AXIS2_PLACEMENT_3D ( 'NONE', #10532, #11456, #939 ) ;
#8959 = ORIENTED_EDGE ( 'NONE', *, *, #456, .T. ) ;
#8960 = DIRECTION ( 'NONE',  ( -1.000000000000000000, 0.000000000000000000, 0.000000000000000000 ) ) ;
#8961 = CIRCLE ( 'NONE', #3126, 15.29705854078138927 ) ;
#8962 = ORIENTED_EDGE ( 'NONE', *, *, #13583, .T. ) ;
#8963 = DIRECTION ( 'NONE',  ( -1.000000000000000000, 0.000000000000000000, 0.000000000000000000 ) ) ;
#8964 = ORIENTED_EDGE ( 'NONE', *, *, #6269, .T. ) ;
#8965 = CARTESIAN_POINT ( 'NONE',  ( 1.718945942447514764E-16, -6.144721277337255927, 1.085069813372578838E-17 ) ) ;
#8966 = DIRECTION ( 'NONE',  ( -1.000000000000000000, 0.000000000000000000, 0.000000000000000000 ) ) ;
#8967 = ADVANCED_FACE ( 'NONE', ( #4833 ), #2208, .F. ) ;
#8968 = DIRECTION ( 'NONE',  ( 0.7999999999999996003, 0.6000000000000007550, 0.000000000000000000 ) ) ;
#8969 = AXIS2_PLACEMENT_3D ( 'NONE', #2162, #4617, #8898 ) ;
#8970 = FACE_OUTER_BOUND ( 'NONE', #3946, .T. ) ;
#8971 = ORIENTED_EDGE ( 'NONE', *, *, #10707, .T. ) ;
#8972 = CIRCLE ( 'NONE', #3574, 10.00000000000000178 ) ;
#8973 = AXIS2_PLACEMENT_3D ( 'NONE', #13492, #11276, #13557 ) ;
#8974 = TOROIDAL_SURFACE ( 'NONE', #10747, 22.99999999999999289, 2.000000000000000000 ) ;
#8975 = ORIENTED_EDGE ( 'NONE', *, *, #5951, .T. ) ;
#8976 = CARTESIAN_POINT ( 'NONE',  ( -10.69346802281034137, -35.22415542633469698, -21.38693604562069694 ) ) ;
#8977 = LINE ( 'NONE', #4843, #12964 ) ;
#8978 = CARTESIAN_POINT ( 'NONE',  ( -9.515638016687521628, -70.53215316236570231, -3.421011903893942829 ) ) ;
#8979 = CARTESIAN_POINT ( 'NONE',  ( 25.00000000000000355, 120.0000000000000284, 2.500000000000000000 ) ) ;
#8980 = CARTESIAN_POINT ( 'NONE',  ( -1.798319979498498977, -80.15852057206338088, -9.967197727661469386 ) ) ;
#8981 = AXIS2_PLACEMENT_3D ( 'NONE', #10412, #13744, #8372 ) ;
#8982 = CARTESIAN_POINT ( 'NONE',  ( 12.99579180576516713, 16.95961992694555676, -25.99158361153032004 ) ) ;
#8983 = AXIS2_PLACEMENT_3D ( 'NONE', #8261, #11416, #8197 ) ;
#8984 = VERTEX_POINT ( 'NONE', #10982 ) ;
#8985 = EDGE_CURVE ( 'NONE', #12700, #7874, #13425, .T. ) ;
#8986 = CARTESIAN_POINT ( 'NONE',  ( 8.385254915620294014, -6.144721277337255039, 16.77050983124059513 ) ) ;
#8987 = EDGE_LOOP ( 'NONE', ( #2547, #4049, #9984, #3615 ) ) ;
#8988 = FACE_OUTER_BOUND ( 'NONE', #7343, .T. ) ;
#8989 = CARTESIAN_POINT ( 'NONE',  ( 19.18070798040252356, 20.00000000000000000, -4.000000000000000000 ) ) ;
#8990 =( BOUNDED_SURFACE ( )  B_SPLINE_SURFACE ( 3, 3, ( 
 ( #11605, #4100, #10553, #8516 ),
 ( #13817, #6282, #13882, #5351 ),
 ( #1091, #7256, #12675, #4165 ),
 ( #9373, #1864, #11672, #7323 ) ),
 .UNSPECIFIED., .F., .F., .T. ) 
 B_SPLINE_SURFACE_WITH_KNOTS ( ( 4, 4 ),
 ( 4, 4 ),
 ( 0.000000000000000000, 1.000000000000000000 ),
 ( 0.000000000000000000, 1.000000000000000000 ),
 .UNSPECIFIED. ) 
 GEOMETRIC_REPRESENTATION_ITEM ( )  RATIONAL_B_SPLINE_SURFACE ( (
 ( 1.000000000000000000, 0.3333333333333334259, 0.3333333333333334259, 1.000000000000000000),
 ( 1.000000000000000000, 0.3333333333333334259, 0.3333333333333334259, 1.000000000000000000),
 ( 1.000000000000000000, 0.3333333333333334259, 0.3333333333333334259, 1.000000000000000000),
 ( 1.000000000000000000, 0.3333333333333334259, 0.3333333333333334259, 1.000000000000000000) ) ) 
 REPRESENTATION_ITEM ( '' )  SURFACE ( )  );
#8991 = ORIENTED_EDGE ( 'NONE', *, *, #9712, .T. ) ;
#8992 = CARTESIAN_POINT ( 'NONE',  ( 5.215657008045057275, -75.40994149440513183, 8.686150177547775186 ) ) ;
#8993 = CARTESIAN_POINT ( 'NONE',  ( 8.385254915620290461, 34.17900274070598243, 2.053795118489799610E-15 ) ) ;
#8994 = AXIS2_PLACEMENT_3D ( 'NONE', #11595, #8501, #12800 ) ;
#8995 = SPHERICAL_SURFACE ( 'NONE', #1877, 5.000000000000000000 ) ;
#8996 = AXIS2_PLACEMENT_3D ( 'NONE', #5549, #6754, #3589 ) ;
#8997 = CARTESIAN_POINT ( 'NONE',  ( 15.29705854078139105, 46.06057977201469100, 3.746698755667522411E-15 ) ) ;
#8998 = CARTESIAN_POINT ( 'NONE',  ( -12.99553232110413781, -17.19957910547634228, -25.99106464220828627 ) ) ;
#8999 = CARTESIAN_POINT ( 'NONE',  ( 2.733214920032663198, -81.93939393936486226, -9.473759075839289778 ) ) ;
#9000 = DIRECTION ( 'NONE',  ( -0.9462100554738961389, -0.3235529800822217195, -1.387852799596036113E-16 ) ) ;
#9001 = CARTESIAN_POINT ( 'NONE',  ( -2.517691654963332357E-15, 90.00000000000000000, -1.589271161308885878E-16 ) ) ;
#9002 = ORIENTED_EDGE ( 'NONE', *, *, #12359, .T. ) ;
#9003 = VERTEX_POINT ( 'NONE', #9171 ) ;
#9004 = DIRECTION ( 'NONE',  ( -0.8000000000000008216, 0.5999999999999988676, 0.000000000000000000 ) ) ;
#9005 = VERTEX_POINT ( 'NONE', #8889 ) ;
#9006 = EDGE_CURVE ( 'NONE', #8407, #8282, #11397, .T. ) ;
#9007 = CARTESIAN_POINT ( 'NONE',  ( -3.317295986488982162, -135.2979454323821358, -0.9176727334396277413 ) ) ;
#9008 = EDGE_CURVE ( 'NONE', #4633, #11439, #2530, .T. ) ;
#9009 = CARTESIAN_POINT ( 'NONE',  ( 28.79177319725820183, -26.24642857144861807, -4.000000000000000000 ) ) ;
#9010 = DIRECTION ( 'NONE',  ( -1.000000000000000000, 0.000000000000000000, 0.000000000000000000 ) ) ;
#9011 = EDGE_CURVE ( 'NONE', #1806, #10192, #11401, .T. ) ;
#9012 = VERTEX_POINT ( 'NONE', #5732 ) ;
#9013 = DIRECTION ( 'NONE',  ( 1.000000000000000000, 0.000000000000000000, 0.000000000000000000 ) ) ;
#9014 = ORIENTED_EDGE ( 'NONE', *, *, #8558, .F. ) ;
#9015 = CARTESIAN_POINT ( 'NONE',  ( 1.692320366844926705, -139.6713384906986448, 2.426530036419475511 ) ) ;
#9016 = DIRECTION ( 'NONE',  ( 1.000000000000000000, 0.000000000000000000, 0.000000000000000000 ) ) ;
#9017 = FACE_BOUND ( 'NONE', #2897, .T. ) ;
#9018 = DIRECTION ( 'NONE',  ( 0.000000000000000000, 0.000000000000000000, 1.000000000000000000 ) ) ;
#9019 = PRODUCT ( 'Pivot Axle Pins', 'Pivot Axle Pins', '', ( #492 ) ) ;
#9020 = DIRECTION ( 'NONE',  ( 0.000000000000000000, 1.000000000000000000, 0.000000000000000000 ) ) ;
#9021 = CARTESIAN_POINT ( 'NONE',  ( 60.49844721164429728, -0.2814068163155458158, -2.499999999999997335 ) ) ;
#9022 = CARTESIAN_POINT ( 'NONE',  ( 15.29705854078139282, 64.91013567203349055, 3.746698755667523989E-15 ) ) ;
#9023 = DIRECTION ( 'NONE',  ( -2.797435172181481150E-17, 1.000000000000000000, -1.765856845898762549E-18 ) ) ;
#9024 = ORIENTED_EDGE ( 'NONE', *, *, #4122, .F. ) ;
#9025 = EDGE_LOOP ( 'NONE', ( #2979, #2052, #12360, #2605 ) ) ;
#9026 = ADVANCED_FACE ( 'NONE', ( #4764 ), #634, .T. ) ;
#9027 = CARTESIAN_POINT ( 'NONE',  ( -4.864544286455551259, -89.44155844152571433, -0.3495895964559158076 ) ) ;
#9028 = ADVANCED_FACE ( 'NONE', ( #8970 ), #13330, .T. ) ;
#9029 = ORIENTED_EDGE ( 'NONE', *, *, #4122, .T. ) ;
#9030 = ADVANCED_FACE ( 'NONE', ( #12548 ), #11615, .T. ) ;
#9031 = CARTESIAN_POINT ( 'NONE',  ( 76.84607712649204814, -99.92541302764922762, 2.500000000000000000 ) ) ;
#9032 = VERTEX_POINT ( 'NONE', #6230 ) ;
#9033 = CARTESIAN_POINT ( 'NONE',  ( -0.2321914886085471308, -147.1038961038843524, 14.56966866480940226 ) ) ;
#9034 = VECTOR ( 'NONE', #9941, 1000.000000000000000 ) ;
#9035 = LINE ( 'NONE', #4889, #2622 ) ;
#9036 = CARTESIAN_POINT ( 'NONE',  ( 8.385254915620299343, -34.41905512736551032, 2.053795118489801582E-15 ) ) ;
#9037 = CARTESIAN_POINT ( 'NONE',  ( -2.517691654963332357E-15, 90.00000000000000000, -1.589271161308885878E-16 ) ) ;
#9038 = ORIENTED_EDGE ( 'NONE', *, *, #1538, .F. ) ;
#9039 = ORIENTED_EDGE ( 'NONE', *, *, #2065, .T. ) ;
#9040 = EDGE_CURVE ( 'NONE', #12557, #8513, #3509, .T. ) ;
#9041 = AXIS2_PLACEMENT_3D ( 'NONE', #11643, #10716, #10591 ) ;
#9042 = DIRECTION ( 'NONE',  ( -0.7328050451781167318, -0.6804386568688601811, -2.313087999326727184E-16 ) ) ;
#9043 = EDGE_CURVE ( 'NONE', #13719, #1890, #9566, .T. ) ;
#9044 = VERTEX_POINT ( 'NONE', #2797 ) ;
#9045 = CARTESIAN_POINT ( 'NONE',  ( 25.00000000000001776, -100.0000000000000000, 7.500000000000000000 ) ) ;
#9046 = DIRECTION ( 'NONE',  ( -1.224646799147353207E-16, 1.000000000000000000, -0.000000000000000000 ) ) ;
#9047 = MECHANICAL_DESIGN_GEOMETRIC_PRESENTATION_REPRESENTATION (  '', ( #5015 ), #12182 ) ;
#9048 = CARTESIAN_POINT ( 'NONE',  ( 42.16244658108818300, 105.4500712252157797, -2.499999999999999556 ) ) ;
#9049 =( BOUNDED_SURFACE ( )  B_SPLINE_SURFACE ( 3, 3, ( 
 ( #5816, #2736, #10234, #7993 ),
 ( #4770, #10097, #8976, #9952 ),
 ( #9116, #13432, #11219, #13505 ),
 ( #1609, #13360, #12272, #7004 ) ),
 .UNSPECIFIED., .F., .F., .F. ) 
 B_SPLINE_SURFACE_WITH_KNOTS ( ( 4, 4 ),
 ( 4, 4 ),
 ( 0.000000000000000000, 1.000000000000000000 ),
 ( 0.000000000000000000, 1.000000000000000000 ),
 .UNSPECIFIED. ) 
 GEOMETRIC_REPRESENTATION_ITEM ( )  RATIONAL_B_SPLINE_SURFACE ( (
 ( 1.000000000000000000, 0.3333333333333334259, 0.3333333333333334259, 1.000000000000000000),
 ( 1.000000000000000000, 0.3333333333333334259, 0.3333333333333334259, 1.000000000000000000),
 ( 1.000000000000000000, 0.3333333333333334259, 0.3333333333333334259, 1.000000000000000000),
 ( 1.000000000000000000, 0.3333333333333334259, 0.3333333333333334259, 1.000000000000000000) ) ) 
 REPRESENTATION_ITEM ( '' )  SURFACE ( )  );
#9050 = CYLINDRICAL_SURFACE ( 'NONE', #815, 2.500000000000000444 ) ;
#9051 = CARTESIAN_POINT ( 'NONE',  ( 3.767919204793307220, -84.38294504924263606, -8.813286018183102755 ) ) ;
#9052 = CARTESIAN_POINT ( 'NONE',  ( -10.69346802281035025, 59.02362407375952102, 21.38693604562068629 ) ) ;
#9053 = AXIS2_PLACEMENT_3D ( 'NONE', #273, #2425, #6706 ) ;
#9054 = ORIENTED_EDGE ( 'NONE', *, *, #2247, .T. ) ;
#9055 = ORIENTED_EDGE ( 'NONE', *, *, #6956, .T. ) ;
#9056 = CARTESIAN_POINT ( 'NONE',  ( -8.621450369311798312, -91.42953101131953986, -1.276853297472915649 ) ) ;
#9057 = CIRCLE ( 'NONE', #3441, 20.00000000000000000 ) ;
#9058 = VERTEX_POINT ( 'NONE', #1804 ) ;
#9059 = CARTESIAN_POINT ( 'NONE',  ( 35.00000000000000000, -4.286263797015736496E-15, 4.000000000000000000 ) ) ;
#9060 = LINE ( 'NONE', #8989, #473 ) ;
#9061 = ORIENTED_EDGE ( 'NONE', *, *, #5450, .T. ) ;
#9062 = CARTESIAN_POINT ( 'NONE',  ( 4.696484759529488962, 90.40938722714874132, 1.719265504264336109 ) ) ;
#9063 = CARTESIAN_POINT ( 'NONE',  ( -2.132246523607266586E-15, 76.22148119144830503, -1.345962243664627229E-16 ) ) ;
#9064 = CARTESIAN_POINT ( 'NONE',  ( 3.371721678969648917, -122.9090909090891728, 4.477688567679800613 ) ) ;
#9065 = CARTESIAN_POINT ( 'NONE',  ( 35.00000000000000000, -4.286263797015736496E-15, 4.000000000000000000 ) ) ;
#9066 = CARTESIAN_POINT ( 'NONE',  ( -1.693173457972974028, -102.5454545454559110, 7.725659299994978468 ) ) ;
#9067 = FACE_OUTER_BOUND ( 'NONE', #2876, .T. ) ;
#9068 = AXIS2_PLACEMENT_3D ( 'NONE', #11824, #9392, #5308 ) ;
#9069 = CARTESIAN_POINT ( 'NONE',  ( 15.70039857998626864, -16.66659488452782156, -0.6827713257413515757 ) ) ;
#9070 = CARTESIAN_POINT ( 'NONE',  ( 34.99999999999958789, 1.063887963769481123E-13, 12.50000000000000000 ) ) ;
#9071 = VECTOR ( 'NONE', #13248, 1000.000000000000000 ) ;
#9072 = ORIENTED_EDGE ( 'NONE', *, *, #4649, .T. ) ;
#9073 = ORIENTED_EDGE ( 'NONE', *, *, #8799, .F. ) ;
#9074 = DIRECTION ( 'NONE',  ( -0.000000000000000000, -0.000000000000000000, -1.000000000000000000 ) ) ;
#9075 = CIRCLE ( 'NONE', #10194, 15.29705854078139105 ) ;
#9076 = ORIENTED_EDGE ( 'NONE', *, *, #211, .T. ) ;
#9077 = CARTESIAN_POINT ( 'NONE',  ( -2.816776700191196081, -98.83340855854847007, -7.314626998258005663 ) ) ;
#9078 = DIRECTION ( 'NONE',  ( -6.158143864569485777E-17, -2.736152283717910599E-16, 1.000000000000000000 ) ) ;
#9079 = CARTESIAN_POINT ( 'NONE',  ( 30.68181818181819054, 131.1340442853780530, -2.499999999999998668 ) ) ;
#9080 = DIRECTION ( 'NONE',  ( -0.9960067511297463483, 0.08927794634716618161, -4.818676322152979407E-17 ) ) ;
#9081 = EDGE_LOOP ( 'NONE', ( #7640, #7991, #3179, #6188 ) ) ;
#9083 = VERTEX_POINT ( 'NONE', #13701 ) ;
#9082 = CIRCLE ( 'NONE', #6833, 35.00000000000000000 ) ;
#9084 = DIRECTION ( 'NONE',  ( 1.000000000000000000, 0.000000000000000000, 0.000000000000000000 ) ) ;
#9085 = ORIENTED_EDGE ( 'NONE', *, *, #3096, .T. ) ;
#9086 = CARTESIAN_POINT ( 'NONE',  ( 2.535732011270894759, -137.7254863561949492, 1.949617200014976071 ) ) ;
#9087 = CARTESIAN_POINT ( 'NONE',  ( 10.00000000000000711, 139.9999999999999716, 0.5000000000000000000 ) ) ;
#9088 = AXIS2_PLACEMENT_3D ( 'NONE', #5405, #4016, #8299 ) ;
#9089 = CARTESIAN_POINT ( 'NONE',  ( 58.17953216333035726, -10.62823074130461620, 2.499999999999998668 ) ) ;
#9090 = EDGE_CURVE ( 'NONE', #8935, #8890, #662, .T. ) ;
#9091 = DIRECTION ( 'NONE',  ( 0.7533101279583152010, -0.6576654553155629745, -1.445602896645893576E-16 ) ) ;
#9092 = DIRECTION ( 'NONE',  ( 0.000000000000000000, -1.000000000000000000, 0.000000000000000000 ) ) ;
#9093 = CARTESIAN_POINT ( 'NONE',  ( 10.69381717166374735, 63.25855867215300066, 21.38763434332750890 ) ) ;
#9094 = DIRECTION ( 'NONE',  ( -1.000000000000000000, 0.000000000000000000, 0.000000000000000000 ) ) ;
#9095 = PRODUCT_DEFINITION_FORMATION_WITH_SPECIFIED_SOURCE ( 'ANY', '', #1387, .NOT_KNOWN. ) ;
#9096 = CARTESIAN_POINT ( 'NONE',  ( -10.43546891138450228, -95.36363636363145702, -7.899666394170180794 ) ) ;
#9097 = CIRCLE ( 'NONE', #2357, 15.29705854078138749 ) ;
#9098 = ORIENTED_EDGE ( 'NONE', *, *, #6026, .F. ) ;
#9099 = DIRECTION ( 'NONE',  ( 0.6000000000000001998, 0.7999999999999998224, -0.000000000000000000 ) ) ;
#9100 = DIRECTION ( 'NONE',  ( -0.000000000000000000, -0.000000000000000000, -1.000000000000000000 ) ) ;
#9101 = ITEM_DEFINED_TRANSFORMATION ( 'NONE', 'NONE', #13619,  #8193 ) ;
#9102 = AXIS2_PLACEMENT_3D ( 'NONE', #1613, #4545, #8904 ) ;
#9103 = CARTESIAN_POINT ( 'NONE',  ( -12.99579180576516713, 35.80917582696438473, -3.253142430666311955E-15 ) ) ;
#9104 = EDGE_CURVE ( 'NONE', #780, #214, #4047, .T. ) ;
#9105 = FACE_OUTER_BOUND ( 'NONE', #5037, .T. ) ;
#9106 = CARTESIAN_POINT ( 'NONE',  ( 12.99579180576516713, -20.73949187309215247, 25.99158361153034491 ) ) ;
#9107 = EDGE_CURVE ( 'NONE', #11721, #4007, #12619, .T. ) ;
#9108 = DIRECTION ( 'NONE',  ( 0.9556796851544554494, -0.2944084567112178474, 0.000000000000000000 ) ) ;
#9109 = DIRECTION ( 'NONE',  ( 1.000000000000000000, 0.000000000000000000, 0.000000000000000000 ) ) ;
#9110 = ADVANCED_FACE ( 'NONE', ( #11551 ), #13763, .T. ) ;
#9111 = EDGE_LOOP ( 'NONE', ( #2361, #2624, #12843, #5769 ) ) ;
#9112 = EDGE_CURVE ( 'NONE', #8398, #4279, #876, .T. ) ;
#9113 = VERTEX_POINT ( 'NONE', #7332 ) ;
#9114 = DIRECTION ( 'NONE',  ( -6.158143864569485777E-17, -2.736152283717910599E-16, 1.000000000000000000 ) ) ;
#9115 = ORIENTED_EDGE ( 'NONE', *, *, #7123, .F. ) ;
#9116 = CARTESIAN_POINT ( 'NONE',  ( 12.99553232110414314, -36.04913500549519512, 1.682098219708385520E-15 ) ) ;
#9117 = FACE_OUTER_BOUND ( 'NONE', #7420, .T. ) ;
#9118 = EDGE_CURVE ( 'NONE', #9823, #7882, #10061, .T. ) ;
#9119 = CARTESIAN_POINT ( 'NONE',  ( -8.558795028186576559, -72.03745728540356197, -5.439008160060279984 ) ) ;
#9120 = CARTESIAN_POINT ( 'NONE',  ( 18.44105126153190710, 8.793532718851094998, -2.499999999999998224 ) ) ;
#9121 = CARTESIAN_POINT ( 'NONE',  ( -4.426053706385205899, -109.9138289782734432, 4.721619936386206362 ) ) ;
#9122 = CARTESIAN_POINT ( 'NONE',  ( 18.54049621773915746, -20.00000000000000000, 7.500000000000000000 ) ) ;
#9123 = VERTEX_POINT ( 'NONE', #7064 ) ;
#9124 = EDGE_CURVE ( 'NONE', #11499, #149, #9821, .T. ) ;
#9125 = ORIENTED_EDGE ( 'NONE', *, *, #4138, .T. ) ;
#9126 = CARTESIAN_POINT ( 'NONE',  ( 8.385254915620297567, -6.144721277337255927, 2.053795118489801582E-15 ) ) ;
#9127 = DIRECTION ( 'NONE',  ( -1.000000000000000000, 0.000000000000000000, 0.000000000000000000 ) ) ;
#9128 = CARTESIAN_POINT ( 'NONE',  ( -0.1768551147989557704, -79.21212121212170132, 10.18346664538817770 ) ) ;
#9129 = ORIENTED_EDGE ( 'NONE', *, *, #9671, .F. ) ;
#9130 = CARTESIAN_POINT ( 'NONE',  ( 6.174202269517973463, -74.54647409589566109, 8.025911141045913411 ) ) ;
#9131 = SURFACE_STYLE_FILL_AREA ( #2679 ) ;
#9132 = CARTESIAN_POINT ( 'NONE',  ( 10.00000000000000711, 139.9999999999999716, 2.500000000000000000 ) ) ;
#9133 = CARTESIAN_POINT ( 'NONE',  ( 34.99999999999958789, 1.104930248025249758E-13, -2.499999999999999112 ) ) ;
#9134 = CARTESIAN_POINT ( 'NONE',  ( 0.2714810715513833461, -148.3982683985791198, 1.717521498777542455 ) ) ;
#9135 = DIRECTION ( 'NONE',  ( 0.9960067511297464593, -0.08927794634716622324, 6.802837160686558945E-17 ) ) ;
#9136 = CARTESIAN_POINT ( 'NONE',  ( 37.50000000000000711, 4.592425496802575156E-15, 7.500000000000000000 ) ) ;
#9137 = CARTESIAN_POINT ( 'NONE',  ( -15.18222645069203125, 20.00000000000000355, 4.000000000000000000 ) ) ;
#9138 = ORIENTED_EDGE ( 'NONE', *, *, #2398, .F. ) ;
#9139 = VERTEX_POINT ( 'NONE', #2859 ) ;
#9140 = CARTESIAN_POINT ( 'NONE',  ( 8.385254915620292238, 15.32944684068712782, 1.002145295323929148E-15 ) ) ;
#9141 = ORIENTED_EDGE ( 'NONE', *, *, #10380, .F. ) ;
#9142 = CARTESIAN_POINT ( 'NONE',  ( -3.045952509441874678, -136.2549498598916671, -1.356822578832249215 ) ) ;
#9143 = CARTESIAN_POINT ( 'NONE',  ( 1.119237408740483274E-15, -40.00941361824966691, 7.065089693818133469E-17 ) ) ;
#9144 = CARTESIAN_POINT ( 'NONE',  ( -39.06230589874905235, 109.5835921350012825, 2.499999999999999556 ) ) ;
#9145 = CYLINDRICAL_SURFACE ( 'NONE', #4046, 15.29705854078139815 ) ;
#9146 = ORIENTED_EDGE ( 'NONE', *, *, #8343, .T. ) ;
#9147 = ORIENTED_EDGE ( 'NONE', *, *, #9804, .F. ) ;
#9148 = CARTESIAN_POINT ( 'NONE',  ( 23.10070469010960537, -97.98123128958475547, -7.500000000000000000 ) ) ;
#9149 = CARTESIAN_POINT ( 'NONE',  ( 3.311736046961211155, -135.3203766226484674, 0.9286747277042636250 ) ) ;
#9150 = FACE_OUTER_BOUND ( 'NONE', #13368, .T. ) ;
#9151 = DIRECTION ( 'NONE',  ( 0.000000000000000000, 0.000000000000000000, 1.000000000000000000 ) ) ;
#9152 = CARTESIAN_POINT ( 'NONE',  ( -38.89115197531750567, 101.6687180808697519, -2.500000000000000000 ) ) ;
#9153 = DIRECTION ( 'NONE',  ( -0.8907235428302473501, 0.4545454545454531425, 0.000000000000000000 ) ) ;
#9154 = CYLINDRICAL_SURFACE ( 'NONE', #9935, 9.000000000008999024 ) ;
#9155 = AXIS2_PLACEMENT_3D ( 'NONE', #7996, #12205, #5968 ) ;
#9156 = ORIENTED_EDGE ( 'NONE', *, *, #133, .F. ) ;
#9157 = CARTESIAN_POINT ( 'NONE',  ( 3.163850051431341015, 90.09728930184206774, 3.875191615614280494 ) ) ;
#9158 = ORIENTED_EDGE ( 'NONE', *, *, #3809, .T. ) ;
#9159 = CARTESIAN_POINT ( 'NONE',  ( 15.29705854078139460, -27.45107625865536605, 1.923489752901240361E-15 ) ) ;
#9160 = ORIENTED_EDGE ( 'NONE', *, *, #1540, .F. ) ;
#9161 = VECTOR ( 'NONE', #4965, 1000.000000000000000 ) ;
#9162 = ORIENTED_EDGE ( 'NONE', *, *, #4890, .F. ) ;
#9163 = DIRECTION ( 'NONE',  ( 1.000000000000000000, 0.000000000000000000, 0.000000000000000000 ) ) ;
#9164 = CARTESIAN_POINT ( 'NONE',  ( -15.64391473689848233, -16.60099851263468196, -1.372939470208868196 ) ) ;
#9165 = CARTESIAN_POINT ( 'NONE',  ( 10.69381717166375800, 34.98422482212468054, -21.38763434332750890 ) ) ;
#9166 = DIRECTION ( 'NONE',  ( -6.158143864569485777E-17, -2.736152283717910599E-16, 1.000000000000000000 ) ) ;
#9167 = DIRECTION ( 'NONE',  ( -6.158143864569485777E-17, -2.736152283717910599E-16, 1.000000000000000000 ) ) ;
#9168 = CARTESIAN_POINT ( 'NONE',  ( -40.74280923682185573, 100.6542365527006098, 1.046903941091061885 ) ) ;
#9169 = CARTESIAN_POINT ( 'NONE',  ( -32.50000000000000000, -3.980102097228898626E-15, 4.000000000000000000 ) ) ;
#9170 = VECTOR ( 'NONE', #5342, 1000.000000000000000 ) ;
#9171 = CARTESIAN_POINT ( 'NONE',  ( -31.81818181818181657, 133.3608531424536920, 0.5000000000000000000 ) ) ;
#9172 = VERTEX_POINT ( 'NONE', #9313 ) ;
#9173 = EDGE_CURVE ( 'NONE', #9032, #3017, #7143, .T. ) ;
#9174 = CARTESIAN_POINT ( 'NONE',  ( -6.361701577163668020, -84.44507371548807839, 7.124205211947466587 ) ) ;
#9175 = EDGE_CURVE ( 'NONE', #11958, #10177, #13894, .T. ) ;
#9176 = VECTOR ( 'NONE', #37, 1000.000000000000000 ) ;
#9177 = ORIENTED_EDGE ( 'NONE', *, *, #5658, .T. ) ;
#9178 = ADVANCED_FACE ( 'NONE', ( #9654, #3263 ), #4443, .T. ) ;
#9179 = CARTESIAN_POINT ( 'NONE',  ( 35.00000000000000000, 4.286263797015736496E-15, -4.000000000000000000 ) ) ;
#9180 = ADVANCED_FACE ( 'NONE', ( #6427 ), #10691, .T. ) ;
#9181 = VECTOR ( 'NONE', #12604, 1000.000000000000000 ) ;
#9182 = CARTESIAN_POINT ( 'NONE',  ( 10.69346802281034670, 77.87317997377837742, 2.619144277183853949E-15 ) ) ;
#9183 = CARTESIAN_POINT ( 'NONE',  ( 37.50000000000002132, 144.4948974278317735, -2.499999999999998668 ) ) ;
#9184 = DIRECTION ( 'NONE',  ( -1.000000000000000000, 0.000000000000000000, 0.000000000000000000 ) ) ;
#9185 = CARTESIAN_POINT ( 'NONE',  ( -5.680349950370690237, -113.5502101303394795, 1.948972962826602595 ) ) ;
#9186 = CARTESIAN_POINT ( 'NONE',  ( 8.385254915620294014, 15.32944684068712782, -16.77050983124058092 ) ) ;
#9187 = VERTEX_POINT ( 'NONE', #13033 ) ;
#9188 = AXIS2_PLACEMENT_3D ( 'NONE', #11074, #5743, #5820 ) ;
#9189 = ORIENTED_EDGE ( 'NONE', *, *, #4368, .T. ) ;
#9190 = DIRECTION ( 'NONE',  ( -2.797435172181481150E-17, 1.000000000000000000, -1.765856845898762549E-18 ) ) ;
#9191 = CIRCLE ( 'NONE', #23, 5.999999999999998224 ) ;
#9192 = VECTOR ( 'NONE', #13075, 1000.000000000000000 ) ;
#9193 = DIRECTION ( 'NONE',  ( -2.797435172181481150E-17, 1.000000000000000000, -1.765856845898762549E-18 ) ) ;
#9194 = ORIENTED_EDGE ( 'NONE', *, *, #11337, .T. ) ;
#9195 = CARTESIAN_POINT ( 'NONE',  ( -8.385254915620295790, -24.99427717735608567, 16.77050983124058448 ) ) ;
#9196 = CARTESIAN_POINT ( 'NONE',  ( 10.14576398710721783, -69.00000000000005684, -0.5510781487875693330 ) ) ;
#9197 = ORIENTED_EDGE ( 'NONE', *, *, #2691, .F. ) ;
#9198 = EDGE_CURVE ( 'NONE', #11053, #6878, #8660, .T. ) ;
#9199 = CARTESIAN_POINT ( 'NONE',  ( 9.567184148105981834, -70.42919439161140360, 3.281027098466867464 ) ) ;
#9200 = FILL_AREA_STYLE_COLOUR ( '', #2356 ) ;
#9201 = EDGE_CURVE ( 'NONE', #2829, #9570, #2345, .T. ) ;
#9202 = AXIS2_PLACEMENT_3D ( 'NONE', #4221, #9633, #8575 ) ;
#9203 = CARTESIAN_POINT ( 'NONE',  ( 21.12690199240172007, 12.61198448588842425, -2.499999999999996447 ) ) ;
#9204 = DIRECTION ( 'NONE',  ( -1.224646799147353207E-16, 1.000000000000000000, -0.000000000000000000 ) ) ;
#9205 = CARTESIAN_POINT ( 'NONE',  ( -0.7374174230184700196, -122.9090909090941182, -5.357146445002623381 ) ) ;
#9206 = FACE_OUTER_BOUND ( 'NONE', #9667, .T. ) ;
#9207 = VECTOR ( 'NONE', #11629, 1000.000000000000114 ) ;
#9208 = DIRECTION ( 'NONE',  ( 0.4545454545454531425, -0.8907235428302472391, 0.000000000000000000 ) ) ;
#9209 =( NAMED_UNIT ( * ) SI_UNIT ( $, .STERADIAN. ) SOLID_ANGLE_UNIT ( ) );
#9210 = VERTEX_POINT ( 'NONE', #5301 ) ;
#9211 = ORIENTED_EDGE ( 'NONE', *, *, #12755, .T. ) ;
#9212 = ORIENTED_EDGE ( 'NONE', *, *, #8153, .T. ) ;
#9213 = ORIENTED_EDGE ( 'NONE', *, *, #2234, .T. ) ;
#9214 = CARTESIAN_POINT ( 'NONE',  ( -2.766560656733045853, -127.7923590214256109, 3.298708284048937678 ) ) ;
#9215 = AXIS2_PLACEMENT_3D ( 'NONE', #3375, #2187, #390 ) ;
#9216 = ADVANCED_FACE ( 'NONE', ( #3394 ), #13828, .T. ) ;
#9217 = FACE_OUTER_BOUND ( 'NONE', #12234, .T. ) ;
#9218 = CIRCLE ( 'NONE', #11444, 2.000000000000003997 ) ;
#9219 = CIRCLE ( 'NONE', #13275, 9.000000000008999024 ) ;
#9220 = LINE ( 'NONE', #739, #3928 ) ;
#9221 = ORIENTED_EDGE ( 'NONE', *, *, #5771, .F. ) ;
#9222 = CARTESIAN_POINT ( 'NONE',  ( -10.00000000000000711, 139.9999999999999716, 0.5000000000000000000 ) ) ;
#9223 = CARTESIAN_POINT ( 'NONE',  ( 0.4876856653298393685, -123.8023944157542928, -4.768975623142601705 ) ) ;
#9224 = EDGE_CURVE ( 'NONE', #5091, #10788, #2207, .T. ) ;
#9225 = DIRECTION ( 'NONE',  ( 0.000000000000000000, 0.000000000000000000, 1.000000000000000000 ) ) ;
#9226 = DIRECTION ( 'NONE',  ( 1.000000000000000000, 3.581364595565021862E-15, 0.000000000000000000 ) ) ;
#9227 = DIRECTION ( 'NONE',  ( 0.000000000000000000, -0.000000000000000000, 1.000000000000000000 ) ) ;
#9228 = DIRECTION ( 'NONE',  ( -0.000000000000000000, -0.000000000000000000, -1.000000000000000000 ) ) ;
#9229 = CARTESIAN_POINT ( 'NONE',  ( 50.00000000000000000, 120.0000000000000284, -0.5000000000000000000 ) ) ;
#9230 = DIRECTION ( 'NONE',  ( -0.000000000000000000, -0.000000000000000000, 1.000000000000000000 ) ) ;
#9231 = CARTESIAN_POINT ( 'NONE',  ( -8.385254915620295790, 50.40394642271930792, -8.900615385087330109E-17 ) ) ;
#9232 = TOROIDAL_SURFACE ( 'NONE', #3160, 77.49999999999998579, 5.000000000000000000 ) ;
#9233 = ORIENTED_EDGE ( 'NONE', *, *, #12026, .T. ) ;
#9234 = CARTESIAN_POINT ( 'NONE',  ( 12.99553232110413781, 39.34908859458022334, 0.000000000000000000 ) ) ;
#9235 = ORIENTED_EDGE ( 'NONE', *, *, #4796, .F. ) ;
#9236 = CARTESIAN_POINT ( 'NONE',  ( -1.315456961488311816, -124.8181818181790845, 4.422452657364224216 ) ) ;
#9237 = ORIENTED_EDGE ( 'NONE', *, *, #9173, .F. ) ;
#9238 = ORIENTED_EDGE ( 'NONE', *, *, #6935, .T. ) ;
#9239 = CARTESIAN_POINT ( 'NONE',  ( -4.769557440008701299, 90.26587002877201371, -1.504714191168455617 ) ) ;
#9240 = CARTESIAN_POINT ( 'NONE',  ( -15.70027825049740500, -16.66645554390144568, -0.3441452025673427118 ) ) ;
#9241 = CARTESIAN_POINT ( 'NONE',  ( 43.63403238902020576, 20.33700654369049587, 2.500000000000006217 ) ) ;
#9242 = CARTESIAN_POINT ( 'NONE',  ( 15.29705854078139105, 8.361467971976955127, 3.746698755667522411E-15 ) ) ;
#9243 = CARTESIAN_POINT ( 'NONE',  ( -21.99999999999999289, -100.0000000000000000, 7.500000000000000000 ) ) ;
#9244 = CARTESIAN_POINT ( 'NONE',  ( -10.69346802281034847, 21.32451227372186864, 21.38693604562068629 ) ) ;
#9245 = DIRECTION ( 'NONE',  ( -1.000000000000000000, 0.000000000000000000, 0.000000000000000000 ) ) ;
#9246 = ORIENTED_EDGE ( 'NONE', *, *, #5666, .T. ) ;
#9247 = EDGE_LOOP ( 'NONE', ( #1389, #6734, #13015, #13863 ) ) ;
#9248 = CARTESIAN_POINT ( 'NONE',  ( -6.048265501886390005, -84.12083291287146380, 7.424871006034148735 ) ) ;
#9249 = ORIENTED_EDGE ( 'NONE', *, *, #560, .F. ) ;
#9250 = ORIENTED_EDGE ( 'NONE', *, *, #2497, .F. ) ;
#9251 = CARTESIAN_POINT ( 'NONE',  ( -15.29705854078139993, -19.91286587805129926, -3.752661754979895291E-15 ) ) ;
#9252 = CARTESIAN_POINT ( 'NONE',  ( 34.63116476221791373, 107.2647840444379028, 2.216888271186473691 ) ) ;
#9253 = CARTESIAN_POINT ( 'NONE',  ( -25.00000000000000355, 120.0000000000000284, 2.500000000000000000 ) ) ;
#9254 = DIRECTION ( 'NONE',  ( 0.000000000000000000, -1.000000000000000000, 0.000000000000000000 ) ) ;
#9255 = CARTESIAN_POINT ( 'NONE',  ( -3.941069743610159826, -121.1799723486271034, -3.201832936236748139 ) ) ;
#9256 = EDGE_CURVE ( 'NONE', #13223, #8652, #1104, .T. ) ;
#9257 = DIRECTION ( 'NONE',  ( 0.000000000000000000, 0.000000000000000000, -1.000000000000000000 ) ) ;
#9258 = EDGE_CURVE ( 'NONE', #11079, #752, #8527, .T. ) ;
#9259 = VECTOR ( 'NONE', #10849, 1000.000000000000000 ) ;
#9260 = ORIENTED_EDGE ( 'NONE', *, *, #11581, .T. ) ;
#9261 = CARTESIAN_POINT ( 'NONE',  ( -3.523137085080624953, 90.23509738553477177, -3.551515709300294255 ) ) ;
#9262 = CIRCLE ( 'NONE', #7018, 8.385254915620294014 ) ;
#9263 = DIRECTION ( 'NONE',  ( 0.8035603370713739757, -0.5952233065713573579, 0.000000000000000000 ) ) ;
#9264 = ORIENTED_EDGE ( 'NONE', *, *, #7538, .T. ) ;
#9265 = FACE_OUTER_BOUND ( 'NONE', #303, .T. ) ;
#9266 = APPLICATION_PROTOCOL_DEFINITION ( 'draft international standard', 'automotive_design', 1998, #11576 ) ;
#9267 = COLOUR_RGB ( '', 0.72549020, 0.75294118, 0.79215686) ;
#9268 = CYLINDRICAL_SURFACE ( 'NONE', #11391, 18.74900000001875000 ) ;
#9269 = CARTESIAN_POINT ( 'NONE',  ( -15.49340857339600319, -22.63585399314533930, -2.623848604783063365 ) ) ;
#9270 = CARTESIAN_POINT ( 'NONE',  ( -2.517691654963332357E-15, 90.00000000000000000, -1.589271161308885878E-16 ) ) ;
#9271 = EDGE_CURVE ( 'NONE', #9823, #10096, #13459, .T. ) ;
#9272 = B_SPLINE_CURVE_WITH_KNOTS ( 'NONE', 3,
 ( #10264, #541, #10338, #1567 ),
 .UNSPECIFIED., .F., .F.,
 ( 4, 4 ),
 ( 0.000000000000000000, 1.000000000000000000 ),
 .UNSPECIFIED. ) ;
#9273 = DIRECTION ( 'NONE',  ( 0.000000000000000000, 0.000000000000000000, 1.000000000000000000 ) ) ;
#9274 = CARTESIAN_POINT ( 'NONE',  ( 35.00000000000001421, -34.99999999999999289, -7.500000000000000000 ) ) ;
#9275 = EDGE_LOOP ( 'NONE', ( #9963, #9639, #12994, #2867 ) ) ;
#9276 = ORIENTED_EDGE ( 'NONE', *, *, #6966, .T. ) ;
#9277 = CARTESIAN_POINT ( 'NONE',  ( -1.937321831943795631E-15, 69.25350232273815720, -1.222917711790730109E-16 ) ) ;
#9278 = EDGE_LOOP ( 'NONE', ( #11872, #11104, #5494, #8971, #515, #2326, #783 ) ) ;
#9279 = EDGE_CURVE ( 'NONE', #6913, #7969, #12749, .T. ) ;
#9280 = VECTOR ( 'NONE', #1056, 1000.000000000000000 ) ;
#9281 = ADVANCED_FACE ( 'NONE', ( #12898 ), #1532, .F. ) ;
#9282 = CARTESIAN_POINT ( 'NONE',  ( -0.8176938719062516459, -100.6571748364077479, -7.534607991170741315 ) ) ;
#9283 = DIRECTION ( 'NONE',  ( 0.4206864060305147146, -0.9072061219927526343, -2.313087999326727677E-16 ) ) ;
#9284 = B_SPLINE_CURVE_WITH_KNOTS ( 'NONE', 3,
 ( #10979, #5728, #993, #2101 ),
 .UNSPECIFIED., .F., .F.,
 ( 4, 4 ),
 ( 0.000000000000000000, 1.000000000000000000 ),
 .UNSPECIFIED. ) ;
#9285 = DIRECTION ( 'NONE',  ( 0.000000000000000000, 0.000000000000000000, 1.000000000000000000 ) ) ;
#9286 = FACE_OUTER_BOUND ( 'NONE', #11650, .T. ) ;
#9287 = CARTESIAN_POINT ( 'NONE',  ( 0.09563759420350162466, -159.7412891347186417, -1.519396412390668250 ) ) ;
#9288 = CIRCLE ( 'NONE', #11739, 4.999999999999997335 ) ;
#9289 = CARTESIAN_POINT ( 'NONE',  ( 1.830305755871358242, -166.5454546033651866, 12.49768923215308192 ) ) ;
#9290 = CARTESIAN_POINT ( 'NONE',  ( 27.45605056404223987, 17.16431845161425684, 2.500000000000004441 ) ) ;
#9291 = VECTOR ( 'NONE', #8790, 1000.000000000000000 ) ;
#9292 = DIRECTION ( 'NONE',  ( 0.7627754036039218200, 0.6466635011015190448, 0.000000000000000000 ) ) ;
#9293 = DIRECTION ( 'NONE',  ( -2.797435172181481150E-17, 1.000000000000000000, -1.765856845898762549E-18 ) ) ;
#9294 = DIRECTION ( 'NONE',  ( 0.000000000000000000, 0.000000000000000000, 1.000000000000000000 ) ) ;
#9295 = AXIS2_PLACEMENT_3D ( 'NONE', #4305, #4233, #10617 ) ;
#9296 = CARTESIAN_POINT ( 'NONE',  ( -10.69346802281035202, 30.74929022373127196, 21.38693604562069339 ) ) ;
#9297 = EDGE_CURVE ( 'NONE', #8022, #1419, #10283, .T. ) ;
#9298 = ORIENTED_EDGE ( 'NONE', *, *, #8666, .T. ) ;
#9299 = DIRECTION ( 'NONE',  ( -1.000000000000000000, -1.601283208593975514E-16, 0.000000000000000000 ) ) ;
#9300 = ORIENTED_EDGE ( 'NONE', *, *, #11526, .F. ) ;
#9301 = CARTESIAN_POINT ( 'NONE',  ( 3.722721133221848611, -134.6363636363726073, -2.741844555831716601 ) ) ;
#9302 = AXIS2_PLACEMENT_3D ( 'NONE', #4653, #4504, #5551 ) ;
#9303 = ORIENTED_EDGE ( 'NONE', *, *, #10941, .F. ) ;
#9304 = CIRCLE ( 'NONE', #6381, 66.24999999999978684 ) ;
#9305 = ORIENTED_EDGE ( 'NONE', *, *, #12889, .T. ) ;
#9306 = DIRECTION ( 'NONE',  ( -1.000000000000000000, 0.000000000000000000, 0.000000000000000000 ) ) ;
#9307 = CYLINDRICAL_SURFACE ( 'NONE', #5945, 4.999999999999997335 ) ;
#9308 = CARTESIAN_POINT ( 'NONE',  ( 15.69972745459287466, -22.78055882083339512, 0.6693078754302104194 ) ) ;
#9309 = DIRECTION ( 'NONE',  ( -1.000000000000000000, 0.000000000000000000, 0.000000000000000000 ) ) ;
#9310 = DIRECTION ( 'NONE',  ( 0.000000000000000000, 0.000000000000000000, 1.000000000000000000 ) ) ;
#9311 = AXIS2_PLACEMENT_3D ( 'NONE', #9481, #6053, #1971 ) ;
#9312 = DIRECTION ( 'NONE',  ( 1.000000000000000000, 1.810146235801886110E-15, 0.000000000000000000 ) ) ;
#9313 = CARTESIAN_POINT ( 'NONE',  ( 57.84299132690245671, 11.33347904398042871, 2.500000000000004441 ) ) ;
#9314 = CIRCLE ( 'NONE', #5267, 24.99999999999998934 ) ;
#9315 = AXIS2_PLACEMENT_3D ( 'NONE', #3092, #4142, #3944 ) ;
#9316 = ORIENTED_EDGE ( 'NONE', *, *, #12876, .T. ) ;
#9317 = EDGE_CURVE ( 'NONE', #297, #10190, #11173, .T. ) ;
#9318 = CIRCLE ( 'NONE', #3049, 15.29705854078139460 ) ;
#9319 = EDGE_LOOP ( 'NONE', ( #5072, #9488, #5667 ) ) ;
#9320 = ORIENTED_EDGE ( 'NONE', *, *, #1232, .T. ) ;
#9321 = CARTESIAN_POINT ( 'NONE',  ( -10.69381717166375090, -21.56444287793185310, -21.38763434332751245 ) ) ;
#9322 = CIRCLE ( 'NONE', #3265, 14.99999999999999112 ) ;
#9323 = CARTESIAN_POINT ( 'NONE',  ( 8.385254915620299343, -34.41905512736551032, 1.085359338644428786E-15 ) ) ;
#9324 = CARTESIAN_POINT ( 'NONE',  ( -45.97632359910779343, 102.2167537197081799, -2.499999999999998668 ) ) ;
#9325 = CARTESIAN_POINT ( 'NONE',  ( 32.50998312217522113, 0.2231948658680255604, 2.500000000000000000 ) ) ;
#9326 = DIRECTION ( 'NONE',  ( 0.000000000000000000, 0.000000000000000000, 1.000000000000000000 ) ) ;
#9327 = CARTESIAN_POINT ( 'NONE',  ( 2.933105132100035206, -136.4276418140068188, -1.575848925487235430 ) ) ;
#9328 = DIRECTION ( 'NONE',  ( -1.000000000000000000, 0.000000000000000000, 0.000000000000000000 ) ) ;
#9329 = VECTOR ( 'NONE', #12459, 1000.000000000000000 ) ;
#9330 = ORIENTED_EDGE ( 'NONE', *, *, #10693, .F. ) ;
#9331 = EDGE_LOOP ( 'NONE', ( #6939, #8786, #6574, #9949 ) ) ;
#9332 = ORIENTED_EDGE ( 'NONE', *, *, #5466, .F. ) ;
#9333 = DIRECTION ( 'NONE',  ( -1.000000000000000000, 0.000000000000000000, 0.000000000000000000 ) ) ;
#9334 = DIRECTION ( 'NONE',  ( -0.000000000000000000, -0.000000000000000000, -1.000000000000000000 ) ) ;
#9335 = EDGE_LOOP ( 'NONE', ( #8818, #7937, #986, #2450 ) ) ;
#9336 = ADVANCED_FACE ( 'NONE', ( #7537 ), #4775, .T. ) ;
#9337 = DIRECTION ( 'NONE',  ( -6.158143864569485777E-17, -2.736152283717910599E-16, 1.000000000000000000 ) ) ;
#9338 = AXIS2_PLACEMENT_3D ( 'NONE', #9940, #3541, #10225 ) ;
#9339 = ORIENTED_EDGE ( 'NONE', *, *, #8775, .T. ) ;
#9340 = CARTESIAN_POINT ( 'NONE',  ( -11.81226048336476886, -40.00941361824966691, -2.803437019582360665E-15 ) ) ;
#9341 = ORIENTED_EDGE ( 'NONE', *, *, #12631, .T. ) ;
#9342 = DIRECTION ( 'NONE',  ( 0.6000000000000001998, -0.7999999999999999334, 0.000000000000000000 ) ) ;
#9343 = CARTESIAN_POINT ( 'NONE',  ( -5.245880486160382716, -97.41991341987385056, -6.871249260548032645 ) ) ;
#9344 = CARTESIAN_POINT ( 'NONE',  ( -1.937321831943795631E-15, 69.25350232273815720, -1.222917711790730109E-16 ) ) ;
#9345 = LINE ( 'NONE', #11514, #1335 ) ;
#9346 = DIRECTION ( 'NONE',  ( -0.000000000000000000, -0.000000000000000000, -1.000000000000000000 ) ) ;
#9347 = CARTESIAN_POINT ( 'NONE',  ( 1.578201174752436931, -125.2149084904265237, 4.340944873416423988 ) ) ;
#9348 = CARTESIAN_POINT ( 'NONE',  ( -35.00000000000000000, -4.286263797015736496E-15, 8.499999999999998224 ) ) ;
#9349 = ORIENTED_EDGE ( 'NONE', *, *, #9849, .F. ) ;
#9350 = ORIENTED_EDGE ( 'NONE', *, *, #13131, .T. ) ;
#9351 = EDGE_LOOP ( 'NONE', ( #9061, #2178, #13246, #10893 ) ) ;
#9352 = DIRECTION ( 'NONE',  ( -6.158143864569485777E-17, -2.736152283717910599E-16, 1.000000000000000000 ) ) ;
#9353 = ADVANCED_FACE ( 'NONE', ( #12251 ), #2496, .T. ) ;
#9354 = CARTESIAN_POINT ( 'NONE',  ( -10.69346802281035025, 40.17406817374067174, 21.38693604562068629 ) ) ;
#9355 = ORIENTED_EDGE ( 'NONE', *, *, #12336, .F. ) ;
#9356 = CARTESIAN_POINT ( 'NONE',  ( 25.00000000000000355, 120.0000000000000284, 2.500000000000000000 ) ) ;
#9357 = ADVANCED_FACE ( 'NONE', ( #6695 ), #1584, .T. ) ;
#9358 = CARTESIAN_POINT ( 'NONE',  ( -1.947123472254133514, -103.3177942292664682, 7.015773985931269330 ) ) ;
#9359 = DIRECTION ( 'NONE',  ( 0.9556796851544554494, -0.2944084567112178474, 0.000000000000000000 ) ) ;
#9360 = DIRECTION ( 'NONE',  ( -2.797435172181481150E-17, 1.000000000000000000, -1.765856845898762549E-18 ) ) ;
#9361 = EDGE_CURVE ( 'NONE', #2743, #7000, #11893, .T. ) ;
#9362 = CARTESIAN_POINT ( 'NONE',  ( 10.69346802281034314, 21.32451227372186864, 1.286451862695887858E-15 ) ) ;
#9363 = EDGE_CURVE ( 'NONE', #11081, #1977, #7803, .T. ) ;
#9364 = CARTESIAN_POINT ( 'NONE',  ( -12.99553232110414491, 1.649976794542511893, -3.188994717863913482E-15 ) ) ;
#9365 = CARTESIAN_POINT ( 'NONE',  ( 25.00000000000002487, -99.43893449056523082, -2.967955073073426764 ) ) ;
#9366 = CARTESIAN_POINT ( 'NONE',  ( 12.99553232110413425, 29.92431064457076673, 25.99106464220827917 ) ) ;
#9367 = DIRECTION ( 'NONE',  ( -1.000000000000000000, 0.000000000000000000, 0.000000000000000000 ) ) ;
#9368 = EDGE_LOOP ( 'NONE', ( #10990, #8408, #11268, #10999 ) ) ;
#9369 = CARTESIAN_POINT ( 'NONE',  ( -10.00000000000000000, 97.99999999999994316, 0.5000000000000000000 ) ) ;
#9370 = DIRECTION ( 'NONE',  ( -1.000000000000000000, 0.000000000000000000, 0.000000000000000000 ) ) ;
#9371 = CARTESIAN_POINT ( 'NONE',  ( -2.518175769240240225, -124.8181818181793403, -12.81633841918550587 ) ) ;
#9372 = ORIENTED_EDGE ( 'NONE', *, *, #9523, .T. ) ;
#9373 = CARTESIAN_POINT ( 'NONE',  ( -8.385254915620294014, -12.94488700934118341, -9.811799245552379678E-16 ) ) ;
#9374 = EDGE_LOOP ( 'NONE', ( #5022, #5199, #9736, #1310 ) ) ;
#9375 = LINE ( 'NONE', #2717, #9538 ) ;
#9376 = DIRECTION ( 'NONE',  ( -1.000000000000000000, -1.224646799147353207E-16, 0.000000000000000000 ) ) ;
#9377 = AXIS2_PLACEMENT_3D ( 'NONE', #11626, #5110, #11566 ) ;
#9378 = CARTESIAN_POINT ( 'NONE',  ( 9.883290025451533012, -72.00000000000005684, 4.866269441041092492 ) ) ;
#9379 = CARTESIAN_POINT ( 'NONE',  ( -6.295302226910096444, -164.3636363587446851, 1.035156591326615194 ) ) ;
#9380 = CIRCLE ( 'NONE', #4666, 69.99999999999998579 ) ;
#9381 = EDGE_CURVE ( 'NONE', #10921, #1460, #1768, .T. ) ;
#9382 = DIRECTION ( 'NONE',  ( 1.000000000000000000, 0.000000000000000000, 0.000000000000000000 ) ) ;
#9383 = DIRECTION ( 'NONE',  ( 1.000000000000000000, -0.000000000000000000, 0.000000000000000000 ) ) ;
#9384 = CARTESIAN_POINT ( 'NONE',  ( -31.81818181818181657, 133.3608531424536920, 0.5000000000000000000 ) ) ;
#9385 = CARTESIAN_POINT ( 'NONE',  ( -4.895553837162441191, 90.06565955263931755, 1.025098571782897539 ) ) ;
#9386 = AXIS2_PLACEMENT_3D ( 'NONE', #13116, #10702, #1183 ) ;
#9387 = ORIENTED_EDGE ( 'NONE', *, *, #7650, .T. ) ;
#9388 = AXIS2_PLACEMENT_3D ( 'NONE', #2889, #450, #1625 ) ;
#9389 = DIRECTION ( 'NONE',  ( -2.797435172181481150E-17, 1.000000000000000000, -1.765856845898762549E-18 ) ) ;
#9390 = EDGE_LOOP ( 'NONE', ( #5533, #5530, #11686, #1431 ) ) ;
#9391 = CARTESIAN_POINT ( 'NONE',  ( 15.29705854078139282, -10.48808792804187284, 1.919277763901059081E-15 ) ) ;
#9392 = DIRECTION ( 'NONE',  ( 0.000000000000000000, 0.000000000000000000, 1.000000000000000000 ) ) ;
#9393 = ADVANCED_FACE ( 'NONE', ( #5717 ), #9856, .T. ) ;
#9394 = CIRCLE ( 'NONE', #3329, 18.74900000001874645 ) ;
#9395 = DIRECTION ( 'NONE',  ( -1.000000000000000000, 0.000000000000000000, -0.000000000000000000 ) ) ;
#9396 = FACE_OUTER_BOUND ( 'NONE', #5130, .T. ) ;
#9397 = CARTESIAN_POINT ( 'NONE',  ( -38.80000000000001137, 101.5999999999999943, -0.5000000000000000000 ) ) ;
#9398 = ORIENTED_EDGE ( 'NONE', *, *, #190, .T. ) ;
#9399 = FACE_OUTER_BOUND ( 'NONE', #4232, .T. ) ;
#9400 = AXIS2_PLACEMENT_3D ( 'NONE', #1653, #5936, #6840 ) ;
#9401 = CARTESIAN_POINT ( 'NONE',  ( 12.99553232110413781, -7.774801155466914970, 25.99106464220828627 ) ) ;
#9402 = CYLINDRICAL_SURFACE ( 'NONE', #11521, 2.500000000000002220 ) ;
#9403 = VECTOR ( 'NONE', #6344, 1000.000000000000000 ) ;
#9404 = ORIENTED_EDGE ( 'NONE', *, *, #9271, .F. ) ;
#9405 = ORIENTED_EDGE ( 'NONE', *, *, #8343, .F. ) ;
#9406 = CARTESIAN_POINT ( 'NONE',  ( 11.81226048336477419, -40.00941361824966691, -23.62452096672953061 ) ) ;
#9407 = ORIENTED_EDGE ( 'NONE', *, *, #4267, .F. ) ;
#9408 = DIRECTION ( 'NONE',  ( -1.000000000000000000, 0.000000000000000000, 0.000000000000000000 ) ) ;
#9409 = CARTESIAN_POINT ( 'NONE',  ( -6.635975953222427393, -85.78354978363292105, 7.919939413296249064 ) ) ;
#9410 = CARTESIAN_POINT ( 'NONE',  ( 50.92330601230504783, -13.90964864522661415, -2.500000000000001776 ) ) ;
#9411 = CARTESIAN_POINT ( 'NONE',  ( -15.36839996672162556, -22.54980054760556385, -3.276782387371333982 ) ) ;
#9412 = CARTESIAN_POINT ( 'NONE',  ( 60.47785218637952198, 1.062566689801823117, -2.499999999999997335 ) ) ;
#9413 = CIRCLE ( 'NONE', #10522, 9.000000000008999024 ) ;
#9414 = CARTESIAN_POINT ( 'NONE',  ( 0.005457668171268584105, -157.8901001905733779, -1.500051909670263139 ) ) ;
#9415 = DIRECTION ( 'NONE',  ( 1.000000000000000000, 0.000000000000000000, 0.000000000000000000 ) ) ;
#9416 = ORIENTED_EDGE ( 'NONE', *, *, #9857, .T. ) ;
#9417 = AXIS2_PLACEMENT_3D ( 'NONE', #2623, #11309, #10125 ) ;
#9418 = ADVANCED_FACE ( 'NONE', ( #4515 ), #3463, .F. ) ;
#9419 = AXIS2_PLACEMENT_3D ( 'NONE', #9807, #215, #4468 ) ;
#9420 = ORIENTED_EDGE ( 'NONE', *, *, #3896, .F. ) ;
#9421 = ORIENTED_EDGE ( 'NONE', *, *, #12107, .T. ) ;
#9422 = CARTESIAN_POINT ( 'NONE',  ( -39.06230589874905235, 109.5835921350012683, -2.499999999999998668 ) ) ;
#9423 = CARTESIAN_POINT ( 'NONE',  ( -15.29705854078139282, 90.00000000000000000, -1.589271161308885878E-16 ) ) ;
#9424 = CIRCLE ( 'NONE', #6277, 2.500000000000002220 ) ;
#9425 = DIRECTION ( 'NONE',  ( 1.000000000000000000, 0.000000000000000000, 0.000000000000000000 ) ) ;
#9426 = CARTESIAN_POINT ( 'NONE',  ( 6.961008101167614370, -85.11900100802145630, -6.453057539919575092 ) ) ;
#9427 = AXIS2_PLACEMENT_3D ( 'NONE', #11135, #3694, #10290 ) ;
#9428 = AXIS2_PLACEMENT_3D ( 'NONE', #3885, #1498, #13467 ) ;
#9429 = CARTESIAN_POINT ( 'NONE',  ( 15.29705854078139282, 64.91013567203349055, 1.757061666260241479E-15 ) ) ;
#9430 = CARTESIAN_POINT ( 'NONE',  ( -35.00000000000000000, -4.286263797015736496E-15, -10.49999999999999822 ) ) ;
#9431 = DIRECTION ( 'NONE',  ( 1.000000000000000000, -1.665334536937735599E-15, 0.000000000000000000 ) ) ;
#9432 = FACE_OUTER_BOUND ( 'NONE', #5198, .T. ) ;
#9433 = CARTESIAN_POINT ( 'NONE',  ( 15.29705854078138572, 66.79670324143890525, 1.757061666260240493E-15 ) ) ;
#9434 = B_SPLINE_CURVE_WITH_KNOTS ( 'NONE', 3,
 ( #5950, #3972, #11336, #13554, #10356, #5092, #9239, #10285, #10222, #3904, #8183, #7193, #2987, #7259 ),
 .UNSPECIFIED., .F., .F.,
 ( 4, 2, 2, 2, 2, 2, 4 ),
 ( 0.000000000000000000, 0.0003997920717328744657, 0.0007995841434657492567, 0.001199376215198623939, 0.001599168286931498947, 0.002398752430397247878, 0.003198336573862997894 ),
 .UNSPECIFIED. ) ;
#9435 = CIRCLE ( 'NONE', #2249, 12.49999999999998757 ) ;
#9436 = EDGE_CURVE ( 'NONE', #9003, #4466, #1313, .T. ) ;
#9437 = CARTESIAN_POINT ( 'NONE',  ( -52.50000000000000000, 120.0000000000000142, 2.499999999999999556 ) ) ;
#9438 = COLOUR_RGB ( '', 0.66274510, 0.83137255, 0.94901961) ;
#9439 = EDGE_LOOP ( 'NONE', ( #8052, #3563, #10284, #9320 ) ) ;
#9440 = DIRECTION ( 'NONE',  ( -1.000000000000000000, 0.000000000000000000, 0.000000000000000000 ) ) ;
#9441 = CIRCLE ( 'NONE', #6299, 18.74900000001875000 ) ;
#9442 = CARTESIAN_POINT ( 'NONE',  ( 2.078065350776520770, -164.3636363707227019, -0.8722068067433885741 ) ) ;
#9443 = ADVANCED_FACE ( 'NONE', ( #3532 ), #494, .T. ) ;
#9444 = VERTEX_POINT ( 'NONE', #9826 ) ;
#9445 = DIRECTION ( 'NONE',  ( -1.000000000000000000, 0.000000000000000000, 0.000000000000000000 ) ) ;
#9446 = VERTEX_POINT ( 'NONE', #10933 ) ;
#9447 = CARTESIAN_POINT ( 'NONE',  ( -8.385254915620292238, -12.94488700934118341, 2.285881734483108495E-17 ) ) ;
#9448 = CARTESIAN_POINT ( 'NONE',  ( -2.517691654963332357E-15, 90.00000000000000000, -1.589271161308885878E-16 ) ) ;
#9449 = CARTESIAN_POINT ( 'NONE',  ( -0.05222919906010464047, -79.03030303040573301, 10.66847369583533833 ) ) ;
#9450 = SHAPE_REPRESENTATION ( 'BR-824', ( #13387, #9990, #8635, #5067, #13619, #4605, #11557, #3473 ), #7287 ) ;
#9451 = CARTESIAN_POINT ( 'NONE',  ( -2.318285725477304826, -147.1038961039276103, -4.595794441988434897 ) ) ;
#9452 = AXIS2_PLACEMENT_3D ( 'NONE', #1108, #4738, #11987 ) ;
#9453 = CARTESIAN_POINT ( 'NONE',  ( 76.84607712649204814, -99.92541302764922762, -2.500000000000000000 ) ) ;
#9454 = DIRECTION ( 'NONE',  ( 0.9960067511297464593, -0.08927794634716622324, 6.802837160686558945E-17 ) ) ;
#9455 = DIRECTION ( 'NONE',  ( 0.8000000000000024869, 0.5999999999999966471, 0.000000000000000000 ) ) ;
#9456 = EDGE_CURVE ( 'NONE', #10190, #3968, #1029, .T. ) ;
#9457 = CARTESIAN_POINT ( 'NONE',  ( 8.385254915620294014, 78.67828027274755698, 8.868043070384791430E-16 ) ) ;
#9458 = ADVANCED_FACE ( 'NONE', ( #7442 ), #10928, .T. ) ;
#9459 = VERTEX_POINT ( 'NONE', #9759 ) ;
#9460 = ADVANCED_FACE ( 'NONE', ( #5538 ), #13472, .F. ) ;
#9461 = EDGE_CURVE ( 'NONE', #988, #534, #12869, .T. ) ;
#9462 = ORIENTED_EDGE ( 'NONE', *, *, #11823, .F. ) ;
#9463 = CARTESIAN_POINT ( 'NONE',  ( -10.69346802281035202, 68.44840202376897764, 21.38693604562068984 ) ) ;
#9464 = CARTESIAN_POINT ( 'NONE',  ( 34.73643445648811934, 107.0738672501280462, 2.329477027598938044 ) ) ;
#9465 = CARTESIAN_POINT ( 'NONE',  ( 10.69381717166375800, -2.714886977913000266, -21.38763434332750890 ) ) ;
#9466 = CARTESIAN_POINT ( 'NONE',  ( 0.1375295535854284268, -156.3065963616199952, 1.553835674430288361 ) ) ;
#9467 = EDGE_CURVE ( 'NONE', #2436, #11706, #8771, .T. ) ;
#9468 = DIRECTION ( 'NONE',  ( -6.158143864569485777E-17, -2.736152283717910599E-16, 1.000000000000000000 ) ) ;
#9469 = ORIENTED_EDGE ( 'NONE', *, *, #11920, .T. ) ;
#9470 = DIRECTION ( 'NONE',  ( -0.6001121574638169642, 0.7999158696163758409, 1.927470528861191270E-16 ) ) ;
#9471 = ADVANCED_FACE ( 'NONE', ( #1271 ), #6467, .T. ) ;
#9472 = CIRCLE ( 'NONE', #13072, 8.385254915620294014 ) ;
#9473 = ORIENTED_EDGE ( 'NONE', *, *, #874, .F. ) ;
#9474 = CYLINDRICAL_SURFACE ( 'NONE', #8161, 15.29705854078139105 ) ;
#9475 = CARTESIAN_POINT ( 'NONE',  ( 9.841115069317121211, -69.87878787878895537, 2.624300023644874802 ) ) ;
#9476 = ORIENTED_EDGE ( 'NONE', *, *, #5265, .T. ) ;
#9477 = CARTESIAN_POINT ( 'NONE',  ( 35.04450421339217314, 112.5597086678580609, -2.499999999999998668 ) ) ;
#9478 = CARTESIAN_POINT ( 'NONE',  ( 1.693173457972444007, -102.5454545454498287, -7.725659299994166673 ) ) ;
#9479 = LINE ( 'NONE', #1061, #9585 ) ;
#9480 = CARTESIAN_POINT ( 'NONE',  ( -15.65828099947304253, -22.75074427536020494, -1.322318745440853593 ) ) ;
#9481 = CARTESIAN_POINT ( 'NONE',  ( -35.00000000000012079, 91.25000000000045475, -4.000000000000000000 ) ) ;
#9482 = DIRECTION ( 'NONE',  ( 1.000000000000000000, -0.000000000000000000, 0.000000000000000000 ) ) ;
#9483 = AXIS2_PLACEMENT_3D ( 'NONE', #7484, #10640, #5312 ) ;
#9484 = CARTESIAN_POINT ( 'NONE',  ( 1.588505082198262697, -106.0776627462951893, -6.756253827230843889 ) ) ;
#9485 = CARTESIAN_POINT ( 'NONE',  ( 50.92330601230504783, -13.90964864522661593, 2.499999999999996891 ) ) ;
#9486 = ORIENTED_EDGE ( 'NONE', *, *, #4473, .F. ) ;
#9487 = ORIENTED_EDGE ( 'NONE', *, *, #2849, .T. ) ;
#9488 = ORIENTED_EDGE ( 'NONE', *, *, #13453, .T. ) ;
#9489 = CARTESIAN_POINT ( 'NONE',  ( 34.99999999999958789, 1.104930248025249758E-13, -2.499999999999999112 ) ) ;
#9490 = FACE_OUTER_BOUND ( 'NONE', #11468, .T. ) ;
#9491 = ORIENTED_EDGE ( 'NONE', *, *, #13419, .F. ) ;
#9492 = CARTESIAN_POINT ( 'NONE',  ( 26.09988479906369463, 19.17858047941126642, 2.500000000000004885 ) ) ;
#9493 = CARTESIAN_POINT ( 'NONE',  ( -2.656653910027198418, -104.0676472691006893, 6.674219718668044088 ) ) ;
#9494 = CARTESIAN_POINT ( 'NONE',  ( 34.25812584745457201, 108.1980041606221050, 0.5000000000000000000 ) ) ;
#9495 = CARTESIAN_POINT ( 'NONE',  ( 0.000000000000000000, -100.0000000000000000, 15.70031846811053455 ) ) ;
#9496 = FACE_OUTER_BOUND ( 'NONE', #83, .T. ) ;
#9497 = CIRCLE ( 'NONE', #11043, 66.25000000000044054 ) ;
#9498 = FACE_OUTER_BOUND ( 'NONE', #1959, .T. ) ;
#9499 = CARTESIAN_POINT ( 'NONE',  ( -8.385254915620299343, 31.55439052270045508, 16.77050983124058803 ) ) ;
#9500 = AXIS2_PLACEMENT_3D ( 'NONE', #10414, #2059, #13876 ) ;
#9501 = CARTESIAN_POINT ( 'NONE',  ( -8.385254915620295790, 50.40394642271930792, -8.900615385087330109E-17 ) ) ;
#9502 = CARTESIAN_POINT ( 'NONE',  ( -24.99999999999998934, -100.0000000000000000, 7.500000000000000000 ) ) ;
#9503 = CARTESIAN_POINT ( 'NONE',  ( 6.075667645224868352, -100.2727272727253762, 11.56208117637901367 ) ) ;
#9504 = EDGE_LOOP ( 'NONE', ( #12058, #12434, #8379, #9138, #4077, #2747 ) ) ;
#9505 = CARTESIAN_POINT ( 'NONE',  ( 36.36363636363638108, 142.2680885707561629, -0.5000000000000000000 ) ) ;
#9506 = ORIENTED_EDGE ( 'NONE', *, *, #1706, .F. ) ;
#9507 = AXIS2_PLACEMENT_3D ( 'NONE', #8884, #3536, #8963 ) ;
#9508 = CARTESIAN_POINT ( 'NONE',  ( -32.50000000000000000, -3.980102097228898626E-15, -7.500000000000000000 ) ) ;
#9509 = CARTESIAN_POINT ( 'NONE',  ( 36.36363636363638108, 142.2680885707561629, 2.500000000000000000 ) ) ;
#9510 = LINE ( 'NONE', #8453, #5818 ) ;
#9511 = CARTESIAN_POINT ( 'NONE',  ( -4.801896836367436805, -140.5584415584283136, -0.8531065430122782844 ) ) ;
#9512 = FACE_OUTER_BOUND ( 'NONE', #12933, .T. ) ;
#9513 = CARTESIAN_POINT ( 'NONE',  ( 8.385254915620288685, -22.36966495935058319, 16.77050983124058448 ) ) ;
#9514 = CARTESIAN_POINT ( 'NONE',  ( -15.29705854078138749, 17.78624592198638155, -3.140796412417860432E-17 ) ) ;
#9515 = DIRECTION ( 'NONE',  ( 0.000000000000000000, 0.000000000000000000, -1.000000000000000000 ) ) ;
#9516 = VERTEX_POINT ( 'NONE', #4415 ) ;
#9517 =( BOUNDED_SURFACE ( )  B_SPLINE_SURFACE ( 3, 3, ( 
 ( #4948, #5790, #8175, #9022 ),
 ( #2710, #553, #10276, #3895 ),
 ( #12393, #12319, #9093, #7892 ),
 ( #13409, #5873, #11327, #678 ) ),
 .UNSPECIFIED., .F., .F., .T. ) 
 B_SPLINE_SURFACE_WITH_KNOTS ( ( 4, 4 ),
 ( 4, 4 ),
 ( 0.000000000000000000, 1.000000000000000000 ),
 ( 0.000000000000000000, 1.000000000000000000 ),
 .UNSPECIFIED. ) 
 GEOMETRIC_REPRESENTATION_ITEM ( )  RATIONAL_B_SPLINE_SURFACE ( (
 ( 1.000000000000000000, 0.3333333333333334259, 0.3333333333333334259, 1.000000000000000000),
 ( 1.000000000000000000, 0.3333333333333334259, 0.3333333333333334259, 1.000000000000000000),
 ( 1.000000000000000000, 0.3333333333333334259, 0.3333333333333334259, 1.000000000000000000),
 ( 1.000000000000000000, 0.3333333333333334259, 0.3333333333333334259, 1.000000000000000000) ) ) 
 REPRESENTATION_ITEM ( '' )  SURFACE ( )  );
#9518 = EDGE_CURVE ( 'NONE', #4518, #6243, #8699, .T. ) ;
#9519 = DIRECTION ( 'NONE',  ( 1.000000000000000000, 0.000000000000000000, 0.000000000000000000 ) ) ;
#9520 = EDGE_LOOP ( 'NONE', ( #6117, #6294, #4645, #13057, #4697, #1828, #1456, #10398, #7099 ) ) ;
#9521 = CARTESIAN_POINT ( 'NONE',  ( -10.69381717166375800, -12.13966492792242846, -2.608463437619201972E-15 ) ) ;
#9522 = AXIS2_PLACEMENT_3D ( 'NONE', #11874, #5488, #7524 ) ;
#9523 = EDGE_CURVE ( 'NONE', #4027, #7120, #8565, .T. ) ;
#9524 = FACE_OUTER_BOUND ( 'NONE', #62, .T. ) ;
#9525 = CARTESIAN_POINT ( 'NONE',  ( 15.29705854078139105, 55.48535772202409078, 3.746698755667522411E-15 ) ) ;
#9526 = AXIS2_PLACEMENT_3D ( 'NONE', #4151, #2053, #13801 ) ;
#9527 = EDGE_CURVE ( 'NONE', #12788, #4855, #7512, .T. ) ;
#9528 = CARTESIAN_POINT ( 'NONE',  ( -9.346811146468073872, -72.85217760321077662, -3.836677974710975825 ) ) ;
#9529 = AXIS2_PLACEMENT_3D ( 'NONE', #3031, #12586, #2893 ) ;
#9530 = EDGE_CURVE ( 'NONE', #13109, #6662, #7582, .T. ) ;
#9531 = CARTESIAN_POINT ( 'NONE',  ( -0.09322702834623840251, -158.9444566874213649, 1.495102636027880738 ) ) ;
#9532 = DIRECTION ( 'NONE',  ( 0.000000000000000000, -1.000000000000000000, 0.000000000000000000 ) ) ;
#9533 = ORIENTED_EDGE ( 'NONE', *, *, #9456, .F. ) ;
#9534 = EDGE_LOOP ( 'NONE', ( #2002, #10233, #8156 ) ) ;
#9535 = VERTEX_POINT ( 'NONE', #5407 ) ;
#9536 = AXIS2_PLACEMENT_3D ( 'NONE', #12150, #4715, #12294 ) ;
#9537 = CARTESIAN_POINT ( 'NONE',  ( 1.387778780781445676E-14, -100.0000000000000000, 0.000000000000000000 ) ) ;
#9538 = VECTOR ( 'NONE', #1593, 1000.000000000000000 ) ;
#9539 = DIRECTION ( 'NONE',  ( -1.000000000000000000, 0.000000000000000000, 0.000000000000000000 ) ) ;
#9540 = EDGE_LOOP ( 'NONE', ( #84, #13297, #12642, #7663 ) ) ;
#9541 = CARTESIAN_POINT ( 'NONE',  ( -12.99553232110414136, 77.04820039461787928, -3.342169200734026966E-15 ) ) ;
#9542 = ORIENTED_EDGE ( 'NONE', *, *, #9635, .T. ) ;
#9543 = CARTESIAN_POINT ( 'NONE',  ( 8.385254915620294014, 12.70483462268159869, 1.002145295323929345E-15 ) ) ;
#9544 = CARTESIAN_POINT ( 'NONE',  ( 35.00000000000000000, 4.286263797015736496E-15, -4.000000000000000000 ) ) ;
#9545 = AXIS2_PLACEMENT_3D ( 'NONE', #5124, #6452, #6582 ) ;
#9546 = CARTESIAN_POINT ( 'NONE',  ( -15.49491024508755999, -22.63688244086937118, 2.616826951557487568 ) ) ;
#9547 = EDGE_CURVE ( 'NONE', #9003, #2436, #1544, .T. ) ;
#9548 = FACE_OUTER_BOUND ( 'NONE', #9319, .T. ) ;
#9549 = CARTESIAN_POINT ( 'NONE',  ( -10.69346802281034314, 68.44840202376897764, -21.38693604562069339 ) ) ;
#9550 = CARTESIAN_POINT ( 'NONE',  ( 5.460914694296556959, -112.4006836749990157, -2.878044288879566537 ) ) ;
#9551 = CARTESIAN_POINT ( 'NONE',  ( -25.00000000000000355, 120.0000000000000142, -0.5000000000000000000 ) ) ;
#9552 = VERTEX_POINT ( 'NONE', #1003 ) ;
#9553 = VERTEX_POINT ( 'NONE', #11720 ) ;
#9554 = EDGE_LOOP ( 'NONE', ( #5234, #999, #5396, #3596 ) ) ;
#9555 = ORIENTED_EDGE ( 'NONE', *, *, #3976, .T. ) ;
#9556 = CARTESIAN_POINT ( 'NONE',  ( 1.344026405355564169, -147.1527166344052944, -1.755549728608237103 ) ) ;
#9557 = CIRCLE ( 'NONE', #8221, 15.70031846811053455 ) ;
#9558 = CARTESIAN_POINT ( 'NONE',  ( 10.69346802281033959, 40.17406817374067174, 21.38693604562069339 ) ) ;
#9559 = CARTESIAN_POINT ( 'NONE',  ( 8.385254915620295790, 40.97916847270985841, -16.77050983124058803 ) ) ;
#9560 = CARTESIAN_POINT ( 'NONE',  ( -4.482662878548983265, -106.3727478091148413, 5.212856551961477791 ) ) ;
#9561 = LINE ( 'NONE', #9495, #896 ) ;
#9562 = EDGE_CURVE ( 'NONE', #1278, #5368, #3038, .T. ) ;
#9563 = CARTESIAN_POINT ( 'NONE',  ( -5.312266725920361310, -76.81818181818026403, -8.563072071058062562 ) ) ;
#9564 = CYLINDRICAL_SURFACE ( 'NONE', #4949, 1.999999999999998224 ) ;
#9565 = CARTESIAN_POINT ( 'NONE',  ( -35.00000000000000000, -4.286263797015736496E-15, 8.499999999999998224 ) ) ;
#9566 = B_SPLINE_CURVE_WITH_KNOTS ( 'NONE', 3,
 ( #1739, #11482, #2994, #10565, #11410, #699, #5101, #2934, #12685, #2011, #967, #10495, #9385, #1876, #6023, #765 ),
 .UNSPECIFIED., .F., .F.,
 ( 4, 2, 2, 2, 2, 2, 2, 4 ),
 ( 0.000000000000000000, 0.0003997740159331186868, 0.0007995480318662373737, 0.001599096063732474747, 0.001998870079665579069, 0.002398644095598683607, 0.002798418111531788145, 0.003198192127464892683 ),
 .UNSPECIFIED. ) ;
#9567 = DIRECTION ( 'NONE',  ( -0.000000000000000000, 0.000000000000000000, -1.000000000000000000 ) ) ;
#9568 = ORIENTED_EDGE ( 'NONE', *, *, #10142, .F. ) ;
#9569 = CARTESIAN_POINT ( 'NONE',  ( 12.05891082652324187, -95.36363636363958562, 5.087868926931951918 ) ) ;
#9570 = VERTEX_POINT ( 'NONE', #3951 ) ;
#9571 = DIRECTION ( 'NONE',  ( -6.158143864569485777E-17, -2.736152283717910599E-16, 1.000000000000000000 ) ) ;
#9572 = ORIENTED_EDGE ( 'NONE', *, *, #3182, .F. ) ;
#9573 = FACE_OUTER_BOUND ( 'NONE', #12918, .T. ) ;
#9574 = CYLINDRICAL_SURFACE ( 'NONE', #3452, 69.99999999999998579 ) ;
#9575 = DIRECTION ( 'NONE',  ( 0.6000000000000001998, -0.7999999999999998224, -0.000000000000000000 ) ) ;
#9576 = CARTESIAN_POINT ( 'NONE',  ( 12.85629483954539509, -68.90909090904808920, -2.086541329743980544 ) ) ;
#9577 =( BOUNDED_SURFACE ( )  B_SPLINE_SURFACE ( 3, 3, ( 
 ( #4789, #1414, #10251, #3501 ),
 ( #3576, #6816, #13451, #1626 ),
 ( #8843, #10118, #8998, #5910 ),
 ( #7940, #387, #2465, #10044 ) ),
 .UNSPECIFIED., .F., .F., .T. ) 
 B_SPLINE_SURFACE_WITH_KNOTS ( ( 4, 4 ),
 ( 4, 4 ),
 ( 0.000000000000000000, 1.000000000000000000 ),
 ( 0.000000000000000000, 1.000000000000000000 ),
 .UNSPECIFIED. ) 
 GEOMETRIC_REPRESENTATION_ITEM ( )  RATIONAL_B_SPLINE_SURFACE ( (
 ( 1.000000000000000000, 0.3333333333333334259, 0.3333333333333334259, 1.000000000000000000),
 ( 1.000000000000000000, 0.3333333333333334259, 0.3333333333333334259, 1.000000000000000000),
 ( 1.000000000000000000, 0.3333333333333334259, 0.3333333333333334259, 1.000000000000000000),
 ( 1.000000000000000000, 0.3333333333333334259, 0.3333333333333334259, 1.000000000000000000) ) ) 
 REPRESENTATION_ITEM ( '' )  SURFACE ( )  );
#9578 = B_SPLINE_CURVE_WITH_KNOTS ( 'NONE', 3,
 ( #13066, #7699, #6654, #7563, #9890, #4624, #1320, #8687, #80, #12925, #1262, #6524, #5527, #291, #4546, #13130 ),
 .UNSPECIFIED., .F., .F.,
 ( 4, 2, 2, 2, 2, 2, 2, 4 ),
 ( 0.000000000000000000, 0.0009977135201011866263, 0.001496570280151776578, 0.001995427040202366747, 0.002494283800252957133, 0.002993140560303546652, 0.003491997320354136604, 0.003990854080404726556 ),
 .UNSPECIFIED. ) ;
#9579 = CARTESIAN_POINT ( 'NONE',  ( -2.517691654963332357E-15, 90.00000000000000000, -1.589271161308885878E-16 ) ) ;
#9580 = DIRECTION ( 'NONE',  ( 2.797435172181480534E-17, -1.000000000000000000, 1.765856845898762164E-18 ) ) ;
#9581 = CYLINDRICAL_SURFACE ( 'NONE', #8571, 40.00000000000001421 ) ;
#9582 = DIRECTION ( 'NONE',  ( 1.000000000000000000, 0.000000000000000000, 0.000000000000000000 ) ) ;
#9583 = EDGE_CURVE ( 'NONE', #3686, #4067, #5271, .T. ) ;
#9584 = ORIENTED_EDGE ( 'NONE', *, *, #12631, .F. ) ;
#9585 = VECTOR ( 'NONE', #10393, 1000.000000000000000 ) ;
#9586 = DIRECTION ( 'NONE',  ( 1.000000000000000000, 0.000000000000000000, 0.000000000000000000 ) ) ;
#9587 = ORIENTED_EDGE ( 'NONE', *, *, #802, .F. ) ;
#9588 = DIRECTION ( 'NONE',  ( 1.000000000000000000, 0.000000000000000000, 0.000000000000000000 ) ) ;
#9589 = CARTESIAN_POINT ( 'NONE',  ( 8.385254915620286909, 69.25350232273815720, 16.77050983124058803 ) ) ;
#9590 = DIRECTION ( 'NONE',  ( -6.158143864569485777E-17, -2.736152283717910599E-16, 1.000000000000000000 ) ) ;
#9591 = CARTESIAN_POINT ( 'NONE',  ( -7.128864053853600780, -75.84752380246891335, -7.199434380052077920 ) ) ;
#9592 = CARTESIAN_POINT ( 'NONE',  ( 1.390017065852572786, -130.6856209220848370, -3.735574746655039746 ) ) ;
#9593 = AXIS2_PLACEMENT_3D ( 'NONE', #8810, #68, #3475 ) ;
#9594 = CARTESIAN_POINT ( 'NONE',  ( -12.99553232110414314, 11.07475474455194053, 25.99106464220826851 ) ) ;
#9595 = AXIS2_PLACEMENT_3D ( 'NONE', #2751, #2818, #13301 ) ;
#9596 = EDGE_LOOP ( 'NONE', ( #7523, #10613, #4538, #3282 ) ) ;
#9597 = EDGE_CURVE ( 'NONE', #3229, #4054, #9394, .T. ) ;
#9598 = ADVANCED_FACE ( 'NONE', ( #7309 ), #8608, .T. ) ;
#9599 = EDGE_LOOP ( 'NONE', ( #10727, #11247, #10354, #5252 ) ) ;
#9600 = ADVANCED_FACE ( 'NONE', ( #9490 ), #3162, .T. ) ;
#9601 = EDGE_CURVE ( 'NONE', #13485, #12269, #1777, .T. ) ;
#9602 = CARTESIAN_POINT ( 'NONE',  ( -2.517691654963332357E-15, 90.00000000000000000, -1.589271161308885878E-16 ) ) ;
#9603 = ORIENTED_EDGE ( 'NONE', *, *, #6097, .F. ) ;
#9604 = ORIENTED_EDGE ( 'NONE', *, *, #61, .T. ) ;
#9605 = CARTESIAN_POINT ( 'NONE',  ( -1.868594470333698657E-15, 66.79670324143890525, -1.179534157023628988E-16 ) ) ;
#9606 = EDGE_LOOP ( 'NONE', ( #10898, #884, #7012, #5248 ) ) ;
#9607 = CYLINDRICAL_SURFACE ( 'NONE', #2721, 5.000000000000000000 ) ;
#9608 = CARTESIAN_POINT ( 'NONE',  ( 8.385254915620292238, 40.97916847270985130, 9.522168693316296019E-16 ) ) ;
#9609 = CYLINDRICAL_SURFACE ( 'NONE', #2700, 66.25000000000044054 ) ;
#9610 = CARTESIAN_POINT ( 'NONE',  ( -24.99999999999998579, -99.15310334213020838, 0.8520627238941246295 ) ) ;
#9611 = CARTESIAN_POINT ( 'NONE',  ( 12.99553232110413958, 67.62342244460847951, -25.99106464220826851 ) ) ;
#9612 = CARTESIAN_POINT ( 'NONE',  ( 2.008006476061143353, -80.00378950643523979, 9.910921260988354575 ) ) ;
#9613 = CARTESIAN_POINT ( 'NONE',  ( 30.45476892764376231, 18.18971895053902443, 2.500000000000004885 ) ) ;
#9614 = EDGE_CURVE ( 'NONE', #5523, #4125, #6256, .T. ) ;
#9615 = VECTOR ( 'NONE', #89, 1000.000000000000000 ) ;
#9616 = VERTEX_POINT ( 'NONE', #10665 ) ;
#9617 = ORIENTED_EDGE ( 'NONE', *, *, #6433, .T. ) ;
#9618 = CIRCLE ( 'NONE', #13486, 69.24999999999975842 ) ;
#9619 = EDGE_CURVE ( 'NONE', #2743, #8621, #5129, .T. ) ;
#9620 = EDGE_CURVE ( 'NONE', #7192, #4098, #2903, .T. ) ;
#9621 = DIRECTION ( 'NONE',  ( -1.000000000000000000, 0.000000000000000000, 0.000000000000000000 ) ) ;
#9622 = ORIENTED_EDGE ( 'NONE', *, *, #6438, .F. ) ;
#9623 = CARTESIAN_POINT ( 'NONE',  ( -25.00000000000000355, 120.0000000000000142, 7.500000000000000000 ) ) ;
#9624 = CARTESIAN_POINT ( 'NONE',  ( 8.406708282432173718, -87.41492670881856952, -3.778913651227076453 ) ) ;
#9625 = DIRECTION ( 'NONE',  ( -1.000000000000000000, -1.224646799147353207E-16, 0.000000000000000000 ) ) ;
#9626 = AXIS2_PLACEMENT_3D ( 'NONE', #10141, #1779, #2708 ) ;
#9627 = CARTESIAN_POINT ( 'NONE',  ( -1.995220113908458437, -142.5800865802677322, -1.459423439931805788 ) ) ;
#9628 = CARTESIAN_POINT ( 'NONE',  ( -10.69381717166375623, 63.25855867215299355, -2.761346882366286462E-15 ) ) ;
#9629 = DIRECTION ( 'NONE',  ( -1.000000000000000000, 0.000000000000000000, 0.000000000000000000 ) ) ;
#9630 = CIRCLE ( 'NONE', #11420, 24.99999999999998934 ) ;
#9631 = CARTESIAN_POINT ( 'NONE',  ( -2.563982627555806637, -78.09090909090801347, -9.749794964675981390 ) ) ;
#9632 = CIRCLE ( 'NONE', #11210, 9.000000000008999024 ) ;
#9633 = DIRECTION ( 'NONE',  ( -2.797435172181481150E-17, 1.000000000000000000, -1.765856845898762549E-18 ) ) ;
#9634 = CARTESIAN_POINT ( 'NONE',  ( 13.79311422413708499, -20.00000000000000355, -7.500000000000000000 ) ) ;
#9635 = EDGE_CURVE ( 'NONE', #2097, #7028, #7153, .T. ) ;
#9636 = VECTOR ( 'NONE', #1954, 1000.000000000000000 ) ;
#9637 = ORIENTED_EDGE ( 'NONE', *, *, #3002, .F. ) ;
#9638 = ADVANCED_FACE ( 'NONE', ( #7240 ), #11655, .T. ) ;
#9639 = ORIENTED_EDGE ( 'NONE', *, *, #8736, .T. ) ;
#9640 = CIRCLE ( 'NONE', #13503, 12.49999999999999289 ) ;
#9641 = CARTESIAN_POINT ( 'NONE',  ( -8.385254915620295790, 69.25350232273815720, -1.222917711790730109E-16 ) ) ;
#9642 = VERTEX_POINT ( 'NONE', #8297 ) ;
#9643 = CARTESIAN_POINT ( 'NONE',  ( 22.00000000000000355, -34.99999999999999289, 7.500000000000000000 ) ) ;
#9644 = FACE_OUTER_BOUND ( 'NONE', #13289, .T. ) ;
#9645 = CARTESIAN_POINT ( 'NONE',  ( 12.99553232110414491, 1.649976794542512559, 3.182987412051232562E-15 ) ) ;
#9646 = CARTESIAN_POINT ( 'NONE',  ( -1.133743435584524839, -129.7272727272675752, 4.472427317383624867 ) ) ;
#9647 = AXIS2_PLACEMENT_3D ( 'NONE', #3753, #7965, #12248 ) ;
#9648 = DIRECTION ( 'NONE',  ( 1.000000000000000000, 3.532527805625498693E-15, 0.000000000000000000 ) ) ;
#9649 = FACE_OUTER_BOUND ( 'NONE', #722, .T. ) ;
#9650 = DIRECTION ( 'NONE',  ( 0.000000000000000000, 0.000000000000000000, 1.000000000000000000 ) ) ;
#9651 = MECHANICAL_DESIGN_GEOMETRIC_PRESENTATION_REPRESENTATION (  '', ( #2476 ), #10757 ) ;
#9652 = DIRECTION ( 'NONE',  ( -2.797435172181481150E-17, 1.000000000000000000, -1.765856845898762549E-18 ) ) ;
#9653 = TOROIDAL_SURFACE ( 'NONE', #3838, 22.99999999999999289, 2.000000000000000000 ) ;
#9654 = FACE_OUTER_BOUND ( 'NONE', #11718, .T. ) ;
#9655 = AXIS2_PLACEMENT_3D ( 'NONE', #10139, #612, #11324 ) ;
#9656 = AXIS2_PLACEMENT_3D ( 'NONE', #8491, #11717, #735 ) ;
#9657 =( LENGTH_UNIT ( ) NAMED_UNIT ( * ) SI_UNIT ( .MILLI., .METRE. ) );
#9658 = ORIENTED_EDGE ( 'NONE', *, *, #13630, .F. ) ;
#9659 = DIRECTION ( 'NONE',  ( 1.000000000000000000, 0.000000000000000000, 0.000000000000000000 ) ) ;
#9660 = CARTESIAN_POINT ( 'NONE',  ( 15.29705854078137861, 66.79670324143890525, 30.59411708156277498 ) ) ;
#9661 = CARTESIAN_POINT ( 'NONE',  ( 12.99579180576516713, 54.65873172698324112, 3.183050967463142985E-15 ) ) ;
#9662 = CARTESIAN_POINT ( 'NONE',  ( -19.38529118556630237, 26.86594603178323482, 5.082853661574513460 ) ) ;
#9663 = CARTESIAN_POINT ( 'NONE',  ( 15.29705854078139815, 0.8232575913728894523, 1.873561326908940224E-15 ) ) ;
#9664 = DIRECTION ( 'NONE',  ( -1.000000000000000000, 0.000000000000000000, 0.000000000000000000 ) ) ;
#9665 = ORIENTED_EDGE ( 'NONE', *, *, #1386, .T. ) ;
#9666 = VERTEX_POINT ( 'NONE', #11523 ) ;
#9667 = EDGE_LOOP ( 'NONE', ( #13734, #9486, #13138, #9934 ) ) ;
#9668 = ORIENTED_EDGE ( 'NONE', *, *, #5433, .F. ) ;
#9669 = DIRECTION ( 'NONE',  ( -6.158143864569485777E-17, -2.736152283717910599E-16, 1.000000000000000000 ) ) ;
#9670 = AXIS2_PLACEMENT_3D ( 'NONE', #9961, #10477, #330 ) ;
#9671 = EDGE_CURVE ( 'NONE', #9709, #11311, #12075, .T. ) ;
#9672 = CARTESIAN_POINT ( 'NONE',  ( -8.385254915620294014, 90.00000000000000000, -1.589271161308885878E-16 ) ) ;
#9673 = EDGE_CURVE ( 'NONE', #3846, #4257, #11622, .T. ) ;
#9674 = DIRECTION ( 'NONE',  ( 1.224646799147353207E-16, -1.000000000000000000, 0.000000000000000000 ) ) ;
#9675 = CARTESIAN_POINT ( 'NONE',  ( 40.81228451836656035, 100.6358150620699803, -0.7758357214534923330 ) ) ;
#9676 = CARTESIAN_POINT ( 'NONE',  ( -60.00000000000001421, 20.00000000000000000, 4.000000000000000000 ) ) ;
#9677 = CARTESIAN_POINT ( 'NONE',  ( -7.874681298106575689, -95.09370015314794955, -2.462075568715513363 ) ) ;
#9678 = PRODUCT_DEFINITION ( 'UNKNOWN', '', #10216, #7986 ) ;
#9679 = CARTESIAN_POINT ( 'NONE',  ( 2.933974605883639275E-16, -10.48808792804187284, 1.852046186812095429E-17 ) ) ;
#9680 = ORIENTED_EDGE ( 'NONE', *, *, #9753, .T. ) ;
#9681 = ORIENTED_EDGE ( 'NONE', *, *, #3809, .F. ) ;
#9682 = EDGE_LOOP ( 'NONE', ( #367, #7905, #9303, #5000 ) ) ;
#9683 = CARTESIAN_POINT ( 'NONE',  ( -4.130090007162179333, 90.90347248489018739, 2.819710018450384048 ) ) ;
#9684 = VERTEX_POINT ( 'NONE', #2312 ) ;
#9685 = DIRECTION ( 'NONE',  ( -6.158143864569485777E-17, -2.736152283717910599E-16, 1.000000000000000000 ) ) ;
#9686 = CARTESIAN_POINT ( 'NONE',  ( 34.25812584745457201, 108.1980041606221050, 0.000000000000000000 ) ) ;
#9687 = ADVANCED_FACE ( 'NONE', ( #2378 ), #7709, .T. ) ;
#9688 = DIRECTION ( 'NONE',  ( -6.158143864569485777E-17, -2.736152283717910599E-16, 1.000000000000000000 ) ) ;
#9689 = AXIS2_PLACEMENT_3D ( 'NONE', #6439, #4455, #2428 ) ;
#9690 = DIRECTION ( 'NONE',  ( 0.7533101279583153120, -0.6576654553155629745, -1.387852799596036359E-16 ) ) ;
#9691 = ADVANCED_FACE ( 'NONE', ( #5468 ), #11005, .T. ) ;
#9692 = CARTESIAN_POINT ( 'NONE',  ( 155.9864723944028810, -111.6214737678657087, 2.500000000000000000 ) ) ;
#9693 = EDGE_CURVE ( 'NONE', #4304, #12949, #12996, .T. ) ;
#9694 = CARTESIAN_POINT ( 'NONE',  ( 0.1768551147990858330, -79.21212121212114710, -10.18346664538823454 ) ) ;
#9695 = CARTESIAN_POINT ( 'NONE',  ( -33.99999999999999289, 108.0000000000000142, -0.5000000000000000000 ) ) ;
#9696 = EDGE_CURVE ( 'NONE', #6030, #4257, #6697, .T. ) ;
#9697 = CARTESIAN_POINT ( 'NONE',  ( 33.39358510189357787, -25.44935030951552690, -6.505213034913026604E-15 ) ) ;
#9698 = AXIS2_PLACEMENT_3D ( 'NONE', #12968, #3336, #7613 ) ;
#9699 = EDGE_CURVE ( 'NONE', #10906, #13516, #7644, .T. ) ;
#9700 = ORIENTED_EDGE ( 'NONE', *, *, #2924, .T. ) ;
#9701 = DIRECTION ( 'NONE',  ( -1.000000000000000000, -2.835060530349834805E-17, 0.000000000000000000 ) ) ;
#9702 = CIRCLE ( 'NONE', #4532, 15.70031846811053455 ) ;
#9703 = CARTESIAN_POINT ( 'NONE',  ( 80.29381926039658879, -64.72749139719506672, 2.500000000000000000 ) ) ;
#9704 = EDGE_LOOP ( 'NONE', ( #7677, #4648, #10813, #2286 ) ) ;
#9705 = DIRECTION ( 'NONE',  ( -1.000000000000000000, -1.224646799147353207E-16, 0.000000000000000000 ) ) ;
#9706 = DIRECTION ( 'NONE',  ( -1.000000000000000000, 0.000000000000000000, 0.000000000000000000 ) ) ;
#9707 = ORIENTED_EDGE ( 'NONE', *, *, #5095, .T. ) ;
#9708 = FACE_OUTER_BOUND ( 'NONE', #3022, .T. ) ;
#9709 = VERTEX_POINT ( 'NONE', #6534 ) ;
#9710 = DIRECTION ( 'NONE',  ( 0.000000000000000000, 0.000000000000000000, 1.000000000000000000 ) ) ;
#9711 = CARTESIAN_POINT ( 'NONE',  ( 15.29705854078138394, 27.21102387199583461, 30.59411708156277854 ) ) ;
#9712 = EDGE_CURVE ( 'NONE', #6075, #973, #10074, .T. ) ;
#9713 = AXIS2_PLACEMENT_3D ( 'NONE', #3507, #10675, #1085 ) ;
#9714 = DIRECTION ( 'NONE',  ( 0.000000000000000000, 0.000000000000000000, -1.000000000000000000 ) ) ;
#9715 = DIRECTION ( 'NONE',  ( -1.000000000000000000, 0.000000000000000000, 0.000000000000000000 ) ) ;
#9716 = CARTESIAN_POINT ( 'NONE',  ( 25.00000000000000355, 120.0000000000000142, 2.500000000000000000 ) ) ;
#9717 = CARTESIAN_POINT ( 'NONE',  ( 0.000000000000000000, 71.01020514433645303, -2.499999999999998668 ) ) ;
#9718 = EDGE_CURVE ( 'NONE', #4393, #5607, #10294, .T. ) ;
#9719 = CARTESIAN_POINT ( 'NONE',  ( 27.38873514654796537, -24.33759740261776017, 4.000000000000000000 ) ) ;
#9720 = DIRECTION ( 'NONE',  ( -1.000000000000000000, 0.000000000000000000, 0.000000000000000000 ) ) ;
#9721 = ORIENTED_EDGE ( 'NONE', *, *, #5335, .T. ) ;
#9722 = EDGE_CURVE ( 'NONE', #11519, #13719, #2861, .T. ) ;
#9723 = AXIS2_PLACEMENT_3D ( 'NONE', #1692, #10583, #8348 ) ;
#9724 = ORIENTED_EDGE ( 'NONE', *, *, #1984, .F. ) ;
#9725 = ORIENTED_EDGE ( 'NONE', *, *, #4851, .T. ) ;
#9726 = DIRECTION ( 'NONE',  ( 0.000000000000000000, 0.000000000000000000, 1.000000000000000000 ) ) ;
#9727 = AXIS2_PLACEMENT_3D ( 'NONE', #8965, #7906, #11896 ) ;
#9728 = CARTESIAN_POINT ( 'NONE',  ( -15.29705854078138927, -38.76242177807012723, 6.844888786042043893E-17 ) ) ;
#9729 = AXIS2_PLACEMENT_3D ( 'NONE', #8519, #2072, #8321 ) ;
#9730 = CARTESIAN_POINT ( 'NONE',  ( -19.96844336951937748, 26.72776445485856200, 1.294012040295340782 ) ) ;
#9731 = DIRECTION ( 'NONE',  ( -1.000000000000000000, 0.000000000000000000, 0.000000000000000000 ) ) ;
#9732 = CARTESIAN_POINT ( 'NONE',  ( 30.72062512117245703, 25.13835616439070719, -4.000000000000000000 ) ) ;
#9733 = AXIS2_PLACEMENT_3D ( 'NONE', #3384, #2271, #1430 ) ;
#9734 = EDGE_LOOP ( 'NONE', ( #7166, #11398, #6485, #13107 ) ) ;
#9735 = B_SPLINE_CURVE_WITH_KNOTS ( 'NONE', 3,
 ( #7535, #6561, #4311, #11039 ),
 .UNSPECIFIED., .F., .F.,
 ( 4, 4 ),
 ( 0.000000000000000000, 1.000000000000000000 ),
 .UNSPECIFIED. ) ;
#9736 = ORIENTED_EDGE ( 'NONE', *, *, #10455, .F. ) ;
#9737 = VECTOR ( 'NONE', #12817, 1000.000000000000000 ) ;
#9738 = ORIENTED_EDGE ( 'NONE', *, *, #2150, .T. ) ;
#9739 = AXIS2_PLACEMENT_3D ( 'NONE', #8714, #469, #10880 ) ;
#9740 = ORIENTED_EDGE ( 'NONE', *, *, #7100, .F. ) ;
#9741 = DIRECTION ( 'NONE',  ( 1.000000000000000000, 1.224646799147353207E-16, 0.000000000000000000 ) ) ;
#9742 = CARTESIAN_POINT ( 'NONE',  ( 22.00000000000002132, -100.0000000000000000, -7.500000000000000000 ) ) ;
#9743 = CARTESIAN_POINT ( 'NONE',  ( -9.175745902881725407E-17, 3.280056672672198914, -5.792110530374064999E-18 ) ) ;
#9744 = CARTESIAN_POINT ( 'NONE',  ( -34.50158885938634512, 107.5319404580926204, -2.003700325319502262 ) ) ;
#9745 = PLANE ( 'NONE',  #3651 ) ;
#9746 = CARTESIAN_POINT ( 'NONE',  ( -4.898028703968604347, -99.35382711894193619, -6.023273615114322688 ) ) ;
#9747 = CYLINDRICAL_SURFACE ( 'NONE', #1027, 2.000000000000000000 ) ;
#9748 = AXIS2_PLACEMENT_3D ( 'NONE', #12442, #605, #1640 ) ;
#9749 = EDGE_LOOP ( 'NONE', ( #7608, #5774, #10976, #5321, #13659 ) ) ;
#9750 = CIRCLE ( 'NONE', #13123, 25.50000000002549783 ) ;
#9751 = EDGE_LOOP ( 'NONE', ( #11467, #11080, #8277, #11833 ) ) ;
#9752 = CIRCLE ( 'NONE', #362, 69.99999999999998579 ) ;
#9753 = EDGE_CURVE ( 'NONE', #973, #2515, #4231, .T. ) ;
#9754 = FACE_OUTER_BOUND ( 'NONE', #281, .T. ) ;
#9755 = LINE ( 'NONE', #8766, #4699 ) ;
#9756 = ORIENTED_EDGE ( 'NONE', *, *, #8331, .F. ) ;
#9757 = CARTESIAN_POINT ( 'NONE',  ( 15.01254563088791372, -15.83514028494776404, -2.500000000000005329 ) ) ;
#9758 = LINE ( 'NONE', #12069, #10840 ) ;
#9759 = CARTESIAN_POINT ( 'NONE',  ( 31.81818181818183433, 133.3608531424536920, 0.5000000000000000000 ) ) ;
#9760 = DIRECTION ( 'NONE',  ( -6.158143864569485777E-17, -2.736152283717910599E-16, 1.000000000000000000 ) ) ;
#9761 =( GEOMETRIC_REPRESENTATION_CONTEXT ( 3 ) GLOBAL_UNCERTAINTY_ASSIGNED_CONTEXT ( ( #698 ) ) GLOBAL_UNIT_ASSIGNED_CONTEXT ( ( #1042, #12966, #13834 ) ) REPRESENTATION_CONTEXT ( 'NONE', 'WORKASPACE' ) );
#9762 = CARTESIAN_POINT ( 'NONE',  ( 23.90723890023449627, -15.11541108221136476, -2.500000000000003553 ) ) ;
#9763 = CIRCLE ( 'NONE', #7515, 17.49999999999999289 ) ;
#9764 = CARTESIAN_POINT ( 'NONE',  ( -7.668969345093498369, -75.54545454545399252, -6.730503492161166612 ) ) ;
#9765 = CARTESIAN_POINT ( 'NONE',  ( 8.385254915620295790, -15.56949922734665570, 2.053795118489800793E-15 ) ) ;
#9766 = CARTESIAN_POINT ( 'NONE',  ( 34.99999999999958789, 1.091249486606660213E-13, 2.500000000000000000 ) ) ;
#9767 = ORIENTED_EDGE ( 'NONE', *, *, #6362, .F. ) ;
#9768 = ADVANCED_FACE ( 'NONE', ( #228 ), #1143, .T. ) ;
#9769 = CARTESIAN_POINT ( 'NONE',  ( 25.00000000000000355, 120.0000000000000284, -2.500000000000000000 ) ) ;
#9770 = DIRECTION ( 'NONE',  ( -0.000000000000000000, -0.000000000000000000, -1.000000000000000000 ) ) ;
#9771 = ORIENTED_EDGE ( 'NONE', *, *, #12755, .F. ) ;
#9772 = EDGE_CURVE ( 'NONE', #1557, #4611, #3552, .T. ) ;
#9773 = B_SPLINE_CURVE_WITH_KNOTS ( 'NONE', 3,
 ( #308, #5410, #6469, #2258 ),
 .UNSPECIFIED., .F., .F.,
 ( 4, 4 ),
 ( 0.000000000000000000, 0.002999984647841453037 ),
 .UNSPECIFIED. ) ;
#9774 = DIRECTION ( 'NONE',  ( 1.000000000000000000, 0.000000000000000000, 0.000000000000000000 ) ) ;
#9775 = DIRECTION ( 'NONE',  ( -1.224646799147353207E-16, 1.000000000000000000, -0.000000000000000000 ) ) ;
#9776 = EDGE_CURVE ( 'NONE', #6151, #5594, #13230, .T. ) ;
#9777 = VERTEX_POINT ( 'NONE', #13143 ) ;
#9778 = CARTESIAN_POINT ( 'NONE',  ( 58.70736094381068426, -9.392073098158828515, 2.499999999999998668 ) ) ;
#9779 = ORIENTED_EDGE ( 'NONE', *, *, #4838, .F. ) ;
#9780 = ADVANCED_FACE ( 'NONE', ( #9754 ), #2455, .T. ) ;
#9781 = CARTESIAN_POINT ( 'NONE',  ( -23.09891356890234348, -97.97864346908494326, -7.500000000000000000 ) ) ;
#9782 = FACE_OUTER_BOUND ( 'NONE', #4326, .T. ) ;
#9783 = TOROIDAL_SURFACE ( 'NONE', #6421, 16.99999999999998934, 2.000000000000000000 ) ;
#9784 = CARTESIAN_POINT ( 'NONE',  ( 1.031578115675553693E-15, -36.87585420866476227, 6.511747960273540061E-17 ) ) ;
#9785 = B_SPLINE_SURFACE_WITH_KNOTS ( 'NONE', 3, 3, ( 
 ( #1620, #3792, #8009, #11298, #8079, #12424, #12362, #10179, #5905, #651, #11364, #7019, #13296, #9196 ),
 ( #522, #721, #588, #2746, #2815, #2532, #1693, #4854, #7857, #7088, #10112, #1757, #4986, #13222 ),
 ( #3569, #12143, #6809, #4783, #444, #11085, #11161, #13375, #1477, #5758, #10036, #7936, #12219, #2608 ),
 ( #6882, #3725, #12285, #9128, #7293, #13848, #6380, #8281, #784, #6313, #5057, #9475, #13650, #10649 ) ),
 .UNSPECIFIED., .F., .F., .F.,
 ( 4, 4 ),
 ( 4, 1, 1, 1, 1, 1, 1, 1, 1, 1, 1, 4 ),
 ( -0.0003000000000000000279, 0.003299999999999999982 ),
 ( 0.07900000000000007017, 0.08000000000000005718, 0.08063636363636368654, 0.08172727272727277337, 0.08336363636363640361, 0.08445454545454547657, 0.08554545454545456340, 0.08663636363636365023, 0.08827272727272726660, 0.08936363636363635343, 0.08999999999999998279, 0.09099999999999996980 ),
 .UNSPECIFIED. ) ;
#9786 = CARTESIAN_POINT ( 'NONE',  ( 12.99579180576516535, 35.80917582696438473, 0.000000000000000000 ) ) ;
#9787 = CARTESIAN_POINT ( 'NONE',  ( 15.29705854078139282, 27.21102387199583461, -30.59411708156277498 ) ) ;
#9788 = DIRECTION ( 'NONE',  ( 1.000000000000000000, 0.000000000000000000, 0.000000000000000000 ) ) ;
#9789 = DIRECTION ( 'NONE',  ( -2.797435172181481150E-17, 1.000000000000000000, -1.765856845898762549E-18 ) ) ;
#9790 = CARTESIAN_POINT ( 'NONE',  ( 25.00000000000000355, 120.0000000000000142, -7.500000000000000000 ) ) ;
#9791 = DIRECTION ( 'NONE',  ( -1.000000000000000000, 0.000000000000000000, 0.000000000000000000 ) ) ;
#9792 = AXIS2_PLACEMENT_3D ( 'NONE', #8036, #5642, #6767 ) ;
#9793 = ORIENTED_EDGE ( 'NONE', *, *, #5840, .T. ) ;
#9794 = DIRECTION ( 'NONE',  ( 6.158143864569485777E-17, 2.736152283717910599E-16, -1.000000000000000000 ) ) ;
#9795 = ORIENTED_EDGE ( 'NONE', *, *, #1370, .T. ) ;
#9796 = ADVANCED_FACE ( 'NONE', ( #165 ), #3724, .F. ) ;
#9797 = VERTEX_POINT ( 'NONE', #1546 ) ;
#9798 = LINE ( 'NONE', #6638, #10407 ) ;
#9799 = DIRECTION ( 'NONE',  ( -0.000000000000000000, -0.000000000000000000, -1.000000000000000000 ) ) ;
#9800 = CARTESIAN_POINT ( 'NONE',  ( 37.50000000000000711, 4.592425496802575156E-15, 7.500000000000000000 ) ) ;
#9801 = CARTESIAN_POINT ( 'NONE',  ( 35.00000000000000000, -4.286263797015736496E-15, -4.000000000000000000 ) ) ;
#9802 = ORIENTED_EDGE ( 'NONE', *, *, #9090, .T. ) ;
#9803 = ORIENTED_EDGE ( 'NONE', *, *, #2929, .F. ) ;
#9804 = EDGE_CURVE ( 'NONE', #4522, #8317, #8276, .T. ) ;
#9805 = ADVANCED_FACE ( 'NONE', ( #12142 ), #3568, .F. ) ;
#9806 = ORIENTED_EDGE ( 'NONE', *, *, #11266, .F. ) ;
#9807 = CARTESIAN_POINT ( 'NONE',  ( 8.894289287455980914E-16, -31.79444290936001138, 5.614443467303076398E-17 ) ) ;
#9808 = ORIENTED_EDGE ( 'NONE', *, *, #6787, .F. ) ;
#9809 = CARTESIAN_POINT ( 'NONE',  ( 15.29705854078139282, 74.33491362204294717, 3.746698755667523989E-15 ) ) ;
#9810 = CIRCLE ( 'NONE', #8257, 9.000000000008999024 ) ;
#9811 = CARTESIAN_POINT ( 'NONE',  ( -31.00000000000000711, -4.286263797015736496E-15, -10.49999999999999822 ) ) ;
#9812 = CARTESIAN_POINT ( 'NONE',  ( -5.215656969546267341, -75.40994152784138294, -8.686150200711136193 ) ) ;
#9813 = CIRCLE ( 'NONE', #11819, 15.29705854078138927 ) ;
#9814 = DIRECTION ( 'NONE',  ( 1.000000000000000000, -2.775557561562892929E-15, 0.000000000000000000 ) ) ;
#9815 = CARTESIAN_POINT ( 'NONE',  ( -10.00000000000000711, 97.99999999999994316, 2.500000000000000000 ) ) ;
#9816 = CARTESIAN_POINT ( 'NONE',  ( 15.29705854078140526, -29.33764382806072746, -30.59411708156279630 ) ) ;
#9817 = DIRECTION ( 'NONE',  ( -1.000000000000000000, 0.000000000000000000, 0.000000000000000000 ) ) ;
#9818 = EDGE_LOOP ( 'NONE', ( #5978, #1089, #4362, #4280 ) ) ;
#9819 = ORIENTED_EDGE ( 'NONE', *, *, #10268, .F. ) ;
#9820 = ORIENTED_EDGE ( 'NONE', *, *, #3508, .T. ) ;
#9821 = CIRCLE ( 'NONE', #13217, 15.29705854078139105 ) ;
#9822 = DIRECTION ( 'NONE',  ( -1.000000000000000000, 0.000000000000000000, 0.000000000000000000 ) ) ;
#9823 = VERTEX_POINT ( 'NONE', #7856 ) ;
#9824 = PLANE ( 'NONE',  #6790 ) ;
#9825 = CARTESIAN_POINT ( 'NONE',  ( 12.99579180576516002, 35.80917582696438473, 25.99158361153033070 ) ) ;
#9826 = CARTESIAN_POINT ( 'NONE',  ( -21.99999999999999289, -97.00000000000000000, -7.500000000000000000 ) ) ;
#9827 = DIRECTION ( 'NONE',  ( 0.000000000000000000, 0.000000000000000000, 1.000000000000000000 ) ) ;
#9828 = LINE ( 'NONE', #4564, #1583 ) ;
#9829 = CARTESIAN_POINT ( 'NONE',  ( -4.858750903447957903, -78.09090909090917876, -8.996753037508826267 ) ) ;
#9830 = EDGE_CURVE ( 'NONE', #2762, #7525, #11957, .T. ) ;
#9831 = VECTOR ( 'NONE', #6461, 1000.000000000000000 ) ;
#9832 = CARTESIAN_POINT ( 'NONE',  ( 12.99553232110414669, -17.19957910547634228, 3.182987412051232956E-15 ) ) ;
#9833 = FILL_AREA_STYLE_COLOUR ( '', #9267 ) ;
#9834 = AXIS2_PLACEMENT_3D ( 'NONE', #4768, #6926, #13429 ) ;
#9835 = ORIENTED_EDGE ( 'NONE', *, *, #8494, .T. ) ;
#9836 = CARTESIAN_POINT ( 'NONE',  ( -19.18070798040252356, 20.00000000000000000, 4.000000000000000000 ) ) ;
#9837 = CARTESIAN_POINT ( 'NONE',  ( 8.385254915620288685, 71.87811454074363837, 9.540301975042856912E-16 ) ) ;
#9838 = ORIENTED_EDGE ( 'NONE', *, *, #6789, .T. ) ;
#9839 = CYLINDRICAL_SURFACE ( 'NONE', #4495, 15.70031846811053455 ) ;
#9840 = DIRECTION ( 'NONE',  ( 0.000000000000000000, 0.000000000000000000, 1.000000000000000000 ) ) ;
#9841 = CIRCLE ( 'NONE', #12767, 69.99999999999998579 ) ;
#9842 = CARTESIAN_POINT ( 'NONE',  ( 1.653273178848927024E-14, -135.0000000000000000, 0.000000000000000000 ) ) ;
#9843 = ORIENTED_EDGE ( 'NONE', *, *, #271, .F. ) ;
#9844 = CARTESIAN_POINT ( 'NONE',  ( -37.50000000000000711, -4.286263797015736496E-15, 4.000000000000000000 ) ) ;
#9845 = CARTESIAN_POINT ( 'NONE',  ( -8.385254915620292238, -31.79444290936001138, 5.614443467303076398E-17 ) ) ;
#9846 = CIRCLE ( 'NONE', #3803, 5.000000000000000000 ) ;
#9847 = CARTESIAN_POINT ( 'NONE',  ( -10.69346802281034847, 2.474956373702985157, -1.318312975903535027E-15 ) ) ;
#9848 = CARTESIAN_POINT ( 'NONE',  ( -35.00000000000000000, -4.286263797015736496E-15, -7.500000000000000000 ) ) ;
#9849 = EDGE_CURVE ( 'NONE', #1947, #3433, #8597, .T. ) ;
#9850 = CYLINDRICAL_SURFACE ( 'NONE', #7614, 4.999999999999993783 ) ;
#9851 = CARTESIAN_POINT ( 'NONE',  ( -10.69346802281034492, 11.89973432371241380, -2.649684675786613482E-15 ) ) ;
#9852 = EDGE_CURVE ( 'NONE', #3741, #7494, #12218, .T. ) ;
#9853 = CARTESIAN_POINT ( 'NONE',  ( -10.69381717166376333, -30.98922082794128485, 21.38763434332751601 ) ) ;
#9854 = CYLINDRICAL_SURFACE ( 'NONE', #13318, 25.50000000002549783 ) ;
#9855 = CIRCLE ( 'NONE', #5367, 25.00000000000000355 ) ;
#9856 = CYLINDRICAL_SURFACE ( 'NONE', #6042, 8.385254915620292238 ) ;
#9857 = EDGE_CURVE ( 'NONE', #2825, #11519, #8008, .T. ) ;
#9858 = AXIS2_PLACEMENT_3D ( 'NONE', #7889, #10272, #4945 ) ;
#9859 = EDGE_LOOP ( 'NONE', ( #2638, #8817, #5702, #3553, #4384, #3344, #2292 ) ) ;
#9860 = CARTESIAN_POINT ( 'NONE',  ( 10.00000000000000711, 139.9999999999999716, 2.500000000000000000 ) ) ;
#9861 = VECTOR ( 'NONE', #7645, 1000.000000000000000 ) ;
#9862 = ORIENTED_EDGE ( 'NONE', *, *, #13760, .F. ) ;
#9863 = VERTEX_POINT ( 'NONE', #10034 ) ;
#9864 = FACE_OUTER_BOUND ( 'NONE', #8751, .T. ) ;
#9865 = AXIS2_PLACEMENT_3D ( 'NONE', #1853, #814, #8309 ) ;
#9866 = PRODUCT_CONTEXT ( 'NONE', #10065, 'mechanical' ) ;
#9867 = ORIENTED_EDGE ( 'NONE', *, *, #7211, .F. ) ;
#9868 = DIRECTION ( 'NONE',  ( 1.000000000000000000, 0.000000000000000000, 0.000000000000000000 ) ) ;
#9869 = EDGE_CURVE ( 'NONE', #6733, #3737, #11297, .T. ) ;
#9870 = CIRCLE ( 'NONE', #8740, 8.385254915620294014 ) ;
#9871 = CARTESIAN_POINT ( 'NONE',  ( 25.00000000000001776, -100.0000000000064801, 5.046127144260958097 ) ) ;
#9872 = ADVANCED_FACE ( 'NONE', ( #6808 ), #845, .T. ) ;
#9873 = CYLINDRICAL_SURFACE ( 'NONE', #4994, 25.00000000000000711 ) ;
#9874 = CARTESIAN_POINT ( 'NONE',  ( 8.385254915620294014, 12.70483462268159869, 2.053795118489800793E-15 ) ) ;
#9875 = EDGE_CURVE ( 'NONE', #5368, #11053, #4330, .T. ) ;
#9876 = ORIENTED_EDGE ( 'NONE', *, *, #11489, .T. ) ;
#9877 = ADVANCED_FACE ( 'NONE', ( #8988 ), #1884, .T. ) ;
#9878 = AXIS2_PLACEMENT_3D ( 'NONE', #3047, #8442, #947 ) ;
#9879 = APPLICATION_CONTEXT ( 'automotive_design' ) ;
#9880 = VERTEX_POINT ( 'NONE', #13295 ) ;
#9881 = AXIS2_PLACEMENT_3D ( 'NONE', #902, #4055, #8336 ) ;
#9882 = CIRCLE ( 'NONE', #11446, 5.000000000000004441 ) ;
#9883 = VERTEX_POINT ( 'NONE', #10178 ) ;
#9884 = DIRECTION ( 'NONE',  ( 2.797435172181480534E-17, -1.000000000000000000, 1.765856845898762164E-18 ) ) ;
#9885 = DIRECTION ( 'NONE',  ( -6.158143864569485777E-17, -2.736152283717910599E-16, 1.000000000000000000 ) ) ;
#9886 = EDGE_CURVE ( 'NONE', #11768, #10108, #4853, .T. ) ;
#9887 = FACE_OUTER_BOUND ( 'NONE', #7626, .T. ) ;
#9888 = VECTOR ( 'NONE', #2775, 1000.000000000000000 ) ;
#9889 = CARTESIAN_POINT ( 'NONE',  ( -8.385254915620294014, -15.56949922734665570, 2.749350679782564022E-17 ) ) ;
#9890 = CARTESIAN_POINT ( 'NONE',  ( 3.286535165834786554, 90.13351245737435136, -3.771524672989932547 ) ) ;
#9891 = DIRECTION ( 'NONE',  ( -1.000000000000000000, 0.000000000000000000, 0.000000000000000000 ) ) ;
#9892 = CARTESIAN_POINT ( 'NONE',  ( 35.00000000000000711, -25.00000000000000000, 7.500000000000000000 ) ) ;
#9893 = VERTEX_POINT ( 'NONE', #4914 ) ;
#9894 = EDGE_CURVE ( 'NONE', #6329, #10788, #2099, .T. ) ;
#9895 = ORIENTED_EDGE ( 'NONE', *, *, #8176, .F. ) ;
#9896 = ORIENTED_EDGE ( 'NONE', *, *, #10630, .T. ) ;
#9897 = PRODUCT ( 'Dual Pivoting Lever Wings (x2)', 'Dual Pivoting Lever Wings (x2)', '', ( #2351 ) ) ;
#9898 = AXIS2_PLACEMENT_3D ( 'NONE', #7384, #7251, #1928 ) ;
#9899 = CARTESIAN_POINT ( 'NONE',  ( -26.79177319725820894, -26.24642857144861807, -4.000000000000000000 ) ) ;
#9900 = ORIENTED_EDGE ( 'NONE', *, *, #6429, .T. ) ;
#9901 = CARTESIAN_POINT ( 'NONE',  ( -8.385254915620292238, -3.520109059331755663, -1.014465541883437468E-15 ) ) ;
#9902 = SURFACE_SIDE_STYLE ('',( #2459 ) ) ;
#9903 = FACE_OUTER_BOUND ( 'NONE', #2127, .T. ) ;
#9904 = DIRECTION ( 'NONE',  ( -1.000000000000000000, 0.000000000000000000, 0.000000000000000000 ) ) ;
#9905 = LINE ( 'NONE', #7653, #9176 ) ;
#9906 = CARTESIAN_POINT ( 'NONE',  ( 0.000000000000000000, 0.000000000000000000, 0.000000000000000000 ) ) ;
#9907 = CARTESIAN_POINT ( 'NONE',  ( 0.000000000000000000, 71.01020514433645303, 7.500000000000000000 ) ) ;
#9908 = DIRECTION ( 'NONE',  ( -1.000000000000000000, 0.000000000000000000, 0.000000000000000000 ) ) ;
#9909 = EDGE_LOOP ( 'NONE', ( #12138, #8556, #6013, #7884 ) ) ;
#9910 = ORIENTED_EDGE ( 'NONE', *, *, #6470, .F. ) ;
#9911 = DIRECTION ( 'NONE',  ( -0.000000000000000000, -0.000000000000000000, -1.000000000000000000 ) ) ;
#9912 = LINE ( 'NONE', #11941, #13814 ) ;
#9913 = CIRCLE ( 'NONE', #8356, 8.385254915620295790 ) ;
#9914 = DIRECTION ( 'NONE',  ( -0.000000000000000000, -0.000000000000000000, -1.000000000000000000 ) ) ;
#9915 = EDGE_LOOP ( 'NONE', ( #10010, #2787, #11177, #5881 ) ) ;
#9916 = AXIS2_PLACEMENT_3D ( 'NONE', #895, #7266, #9312 ) ;
#9917 = ORIENTED_EDGE ( 'NONE', *, *, #2590, .T. ) ;
#9918 = CYLINDRICAL_SURFACE ( 'NONE', #1912, 10.00000000000000178 ) ;
#9919 = ORIENTED_EDGE ( 'NONE', *, *, #27, .T. ) ;
#9920 = DIRECTION ( 'NONE',  ( -0.000000000000000000, -0.000000000000000000, -1.000000000000000000 ) ) ;
#9921 = CYLINDRICAL_SURFACE ( 'NONE', #675, 15.29705854078139105 ) ;
#9922 = CARTESIAN_POINT ( 'NONE',  ( 42.49999999999999289, 120.0000000000000142, 7.500000000000000000 ) ) ;
#9923 = CARTESIAN_POINT ( 'NONE',  ( -35.00000000000000000, -20.00000000000000000, -7.500000000000000000 ) ) ;
#9924 = FACE_OUTER_BOUND ( 'NONE', #13398, .T. ) ;
#9925 = CARTESIAN_POINT ( 'NONE',  ( 8.385254915620292238, -31.79444290936001494, 16.77050983124058803 ) ) ;
#9926 = CARTESIAN_POINT ( 'NONE',  ( -1.747091603990086329E-15, 62.45333659073423860, -1.102836519679677113E-16 ) ) ;
#9927 = VECTOR ( 'NONE', #2103, 1000.000000000000000 ) ;
#9928 = CARTESIAN_POINT ( 'NONE',  ( -32.72727272727271952, 135.1423002281141805, 0.5000000000000000000 ) ) ;
#9929 = VERTEX_POINT ( 'NONE', #7345 ) ;
#9930 = DIRECTION ( 'NONE',  ( -2.797435172181481150E-17, 1.000000000000000000, -1.765856845898762549E-18 ) ) ;
#9931 = VERTEX_POINT ( 'NONE', #2879 ) ;
#9932 = EDGE_CURVE ( 'NONE', #8652, #7028, #11060, .T. ) ;
#9933 = CIRCLE ( 'NONE', #2990, 5.000000000000000000 ) ;
#9934 = ORIENTED_EDGE ( 'NONE', *, *, #5513, .T. ) ;
#9935 = AXIS2_PLACEMENT_3D ( 'NONE', #8952, #13258, #3825 ) ;
#9936 = FACE_OUTER_BOUND ( 'NONE', #9081, .T. ) ;
#9937 = ORIENTED_EDGE ( 'NONE', *, *, #2420, .F. ) ;
#9938 = PRODUCT_RELATED_PRODUCT_CATEGORY ( 'part', '', ( #9897 ) ) ;
#9939 = DIRECTION ( 'NONE',  ( -0.000000000000000000, -0.000000000000000000, -1.000000000000000000 ) ) ;
#9940 = CARTESIAN_POINT ( 'NONE',  ( 35.00000000000000000, 4.286263797015736496E-15, 7.500000000000000000 ) ) ;
#9941 = DIRECTION ( 'NONE',  ( 0.000000000000000000, -1.000000000000000000, 0.000000000000000000 ) ) ;
#9942 = CARTESIAN_POINT ( 'NONE',  ( 5.049283658538309183, -77.73593556436266283, 8.777051982195970936 ) ) ;
#9943 = AXIS2_PLACEMENT_3D ( 'NONE', #2745, #5684, #1619 ) ;
#9944 = ORIENTED_EDGE ( 'NONE', *, *, #7288, .F. ) ;
#9945 = ORIENTED_EDGE ( 'NONE', *, *, #7461, .T. ) ;
#9946 = ADVANCED_FACE ( 'NONE', ( #6311 ), #5235, .F. ) ;
#9947 = B_SPLINE_CURVE_WITH_KNOTS ( 'NONE', 3,
 ( #3654, #2614, #3798, #8085 ),
 .UNSPECIFIED., .F., .F.,
 ( 4, 4 ),
 ( 0.000000000000000000, 1.000000000000000000 ),
 .UNSPECIFIED. ) ;
#9948 = ADVANCED_FACE ( 'NONE', ( #7154 ), #1755, .F. ) ;
#9949 = ORIENTED_EDGE ( 'NONE', *, *, #207, .F. ) ;
#9950 = CARTESIAN_POINT ( 'NONE',  ( 32.72727272727274084, 135.1423002281142089, -2.500000000000000000 ) ) ;
#9951 = EDGE_CURVE ( 'NONE', #13265, #1727, #3413, .T. ) ;
#9952 = CARTESIAN_POINT ( 'NONE',  ( -10.69346802281034670, -35.22415542633469698, -2.569297226391742986E-15 ) ) ;
#9953 = AXIS2_PLACEMENT_3D ( 'NONE', #404, #7802, #12091 ) ;
#9954 = EDGE_CURVE ( 'NONE', #2529, #13355, #264, .T. ) ;
#9955 = FACE_OUTER_BOUND ( 'NONE', #7929, .T. ) ;
#9956 = CYLINDRICAL_SURFACE ( 'NONE', #4041, 18.74900000001875000 ) ;
#9957 = DIRECTION ( 'NONE',  ( 1.000000000000000000, 0.000000000000000000, 0.000000000000000000 ) ) ;
#9958 = CARTESIAN_POINT ( 'NONE',  ( -2.517691654963332357E-15, 90.00000000000000000, -1.589271161308885878E-16 ) ) ;
#9959 = CARTESIAN_POINT ( 'NONE',  ( 10.69346802281034314, 59.02362407375952102, 2.619144277183853160E-15 ) ) ;
#9960 = ORIENTED_EDGE ( 'NONE', *, *, #8397, .F. ) ;
#9961 = CARTESIAN_POINT ( 'NONE',  ( 32.72727272727274084, 135.1423002281141805, 0.5000000000000000000 ) ) ;
#9962 = ORIENTED_EDGE ( 'NONE', *, *, #4796, .T. ) ;
#9963 = ORIENTED_EDGE ( 'NONE', *, *, #1457, .F. ) ;
#9964 = AXIS2_PLACEMENT_3D ( 'NONE', #7795, #1426, #401 ) ;
#9965 = TOROIDAL_SURFACE ( 'NONE', #13595, 48.00000000000001421, 2.000000000000000000 ) ;
#9966 = CARTESIAN_POINT ( 'NONE',  ( -10.00000000000000000, 92.00000000000000000, -0.5000000000000000000 ) ) ;
#9967 = CARTESIAN_POINT ( 'NONE',  ( -29.00000000000000355, -5.021051876504148963E-15, -7.500000000000000000 ) ) ;
#9968 =( BOUNDED_SURFACE ( )  B_SPLINE_SURFACE ( 3, 3, ( 
 ( #11058, #7910, #13277, #7063 ),
 ( #3698, #9244, #12262, #11343 ),
 ( #6860, #4891, #1738, #13424 ),
 ( #13559, #5807, #10013, #501 ) ),
 .UNSPECIFIED., .F., .F., .F. ) 
 B_SPLINE_SURFACE_WITH_KNOTS ( ( 4, 4 ),
 ( 4, 4 ),
 ( 0.000000000000000000, 1.000000000000000000 ),
 ( 0.000000000000000000, 1.000000000000000000 ),
 .UNSPECIFIED. ) 
 GEOMETRIC_REPRESENTATION_ITEM ( )  RATIONAL_B_SPLINE_SURFACE ( (
 ( 1.000000000000000000, 0.3333333333333334259, 0.3333333333333334259, 1.000000000000000000),
 ( 1.000000000000000000, 0.3333333333333334259, 0.3333333333333334259, 1.000000000000000000),
 ( 1.000000000000000000, 0.3333333333333334259, 0.3333333333333334259, 1.000000000000000000),
 ( 1.000000000000000000, 0.3333333333333334259, 0.3333333333333334259, 1.000000000000000000) ) ) 
 REPRESENTATION_ITEM ( '' )  SURFACE ( )  );
#9969 = ORIENTED_EDGE ( 'NONE', *, *, #5674, .F. ) ;
#9970 = DIRECTION ( 'NONE',  ( -6.158143864569485777E-17, -2.736152283717910599E-16, 1.000000000000000000 ) ) ;
#9971 = DIRECTION ( 'NONE',  ( -0.000000000000000000, -0.000000000000000000, -1.000000000000000000 ) ) ;
#9972 = EDGE_CURVE ( 'NONE', #2032, #12858, #8278, .T. ) ;
#9973 = DIRECTION ( 'NONE',  ( -1.000000000000000000, 0.000000000000000000, 0.000000000000000000 ) ) ;
#9974 = CARTESIAN_POINT ( 'NONE',  ( 5.494716852924988792, -106.9090909090932087, -4.862358660864441795 ) ) ;
#9975 = FACE_OUTER_BOUND ( 'NONE', #10386, .T. ) ;
#9976 = CARTESIAN_POINT ( 'NONE',  ( 2.179449471770333435, 90.00000000000000000, 4.500000000000000888 ) ) ;
#9977 = AXIS2_PLACEMENT_3D ( 'NONE', #6481, #3311, #1162 ) ;
#9978 = CARTESIAN_POINT ( 'NONE',  ( 6.213657885906443745, -97.41991341991004560, 5.968417174470181941 ) ) ;
#9979 = DIRECTION ( 'NONE',  ( -6.158143864569485777E-17, -2.736152283717910599E-16, 1.000000000000000000 ) ) ;
#9980 = CARTESIAN_POINT ( 'NONE',  ( 15.29705854078139637, -18.02629830864593785, 3.746698755667523989E-15 ) ) ;
#9981 = AXIS2_PLACEMENT_3D ( 'NONE', #609, #2702, #6977 ) ;
#9982 = PRESENTATION_STYLE_ASSIGNMENT (( #10256 ) ) ;
#9983 = AXIS2_PLACEMENT_3D ( 'NONE', #9551, #8154, #11372 ) ;
#9984 = ORIENTED_EDGE ( 'NONE', *, *, #7375, .T. ) ;
#9985 = ORIENTED_EDGE ( 'NONE', *, *, #8570, .T. ) ;
#9986 = CARTESIAN_POINT ( 'NONE',  ( -22.00000000000000000, -2.694222958124176809E-15, 0.000000000000000000 ) ) ;
#9987 = DIRECTION ( 'NONE',  ( -1.224646799147353207E-16, -1.499759782661857608E-32, 1.000000000000000000 ) ) ;
#9988 = VECTOR ( 'NONE', #290, 1000.000000000000000 ) ;
#9989 = DIRECTION ( 'NONE',  ( -6.158143864569485777E-17, -2.736152283717910599E-16, 1.000000000000000000 ) ) ;
#9990 = AXIS2_PLACEMENT_3D ( 'NONE', #3199, #5236, #9519 ) ;
#9991 = DIRECTION ( 'NONE',  ( -1.000000000000000000, 0.000000000000000000, 0.000000000000000000 ) ) ;
#9992 = ORIENTED_EDGE ( 'NONE', *, *, #4629, .T. ) ;
#9993 = DIRECTION ( 'NONE',  ( -0.000000000000000000, -0.000000000000000000, -1.000000000000000000 ) ) ;
#9994 = AXIS2_PLACEMENT_3D ( 'NONE', #11271, #1666, #12467 ) ;
#9995 = DIRECTION ( 'NONE',  ( -2.797435172181481150E-17, 1.000000000000000000, -1.765856845898762549E-18 ) ) ;
#9996 = EDGE_CURVE ( 'NONE', #5217, #7956, #851, .T. ) ;
#9997 = DIRECTION ( 'NONE',  ( -2.797435172181481150E-17, 1.000000000000000000, -1.765856845898762549E-18 ) ) ;
#9998 = DIRECTION ( 'NONE',  ( -6.158143864569485777E-17, -2.736152283717910599E-16, 1.000000000000000000 ) ) ;
#9999 = LINE ( 'NONE', #8719, #2467 ) ;
#10000 = CARTESIAN_POINT ( 'NONE',  ( 25.00000000000000355, 120.0000000000000142, 0.5000000000000000000 ) ) ;
#10001 = DIRECTION ( 'NONE',  ( -6.158143864569485777E-17, -2.736152283717910599E-16, 1.000000000000000000 ) ) ;
#10002 = CARTESIAN_POINT ( 'NONE',  ( -21.99999999999999289, -100.0000000000000000, -7.500000000000000000 ) ) ;
#10003 = CIRCLE ( 'NONE', #381, 82.49999999999998579 ) ;
#10004 = CARTESIAN_POINT ( 'NONE',  ( 34.99999999999958789, 1.091249486606660213E-13, 2.500000000000000000 ) ) ;
#10005 = CARTESIAN_POINT ( 'NONE',  ( 10.69346802281034847, -6.949821576306441706, 1.321354522272860754E-15 ) ) ;
#10006 = ORIENTED_EDGE ( 'NONE', *, *, #950, .F. ) ;
#10007 = VECTOR ( 'NONE', #9383, 1000.000000000000000 ) ;
#10008 = ORIENTED_EDGE ( 'NONE', *, *, #636, .F. ) ;
#10009 = CARTESIAN_POINT ( 'NONE',  ( 34.99999999999999289, 25.00000000000002132, 7.500000000000000000 ) ) ;
#10010 = ORIENTED_EDGE ( 'NONE', *, *, #12641, .T. ) ;
#10011 = CARTESIAN_POINT ( 'NONE',  ( 55.20422767451771051, -6.230504303137470501, -2.499999999999999112 ) ) ;
#10012 = DIRECTION ( 'NONE',  ( -0.000000000000000000, -0.000000000000000000, -1.000000000000000000 ) ) ;
#10013 = CARTESIAN_POINT ( 'NONE',  ( 15.29705854078138394, 19.67281349139177138, 30.59411708156277854 ) ) ;
#10014 = ADVANCED_FACE ( 'NONE', ( #13648 ), #918, .T. ) ;
#10015 = DIRECTION ( 'NONE',  ( -2.797435172181481150E-17, 1.000000000000000000, -1.765856845898762549E-18 ) ) ;
#10016 = PRODUCT ( 'Threaded Steel Worm Screw Spindle', 'Threaded Steel Worm Screw Spindle', '', ( #9866 ) ) ;
#10017 = ORIENTED_EDGE ( 'NONE', *, *, #7567, .T. ) ;
#10018 = CARTESIAN_POINT ( 'NONE',  ( 10.69346802281034847, -25.79937747632526879, 1.362902637283517672E-15 ) ) ;
#10019 = VECTOR ( 'NONE', #9482, 1000.000000000000000 ) ;
#10020 = ORIENTED_EDGE ( 'NONE', *, *, #1895, .F. ) ;
#10021 = VERTEX_POINT ( 'NONE', #8415 ) ;
#10022 =( NAMED_UNIT ( * ) PLANE_ANGLE_UNIT ( ) SI_UNIT ( $, .RADIAN. ) );
#10023 = CARTESIAN_POINT ( 'NONE',  ( 1.187907395172932673E-14, -97.00000000000000000, 0.000000000000000000 ) ) ;
#10024 = FACE_OUTER_BOUND ( 'NONE', #3648, .T. ) ;
#10025 = CARTESIAN_POINT ( 'NONE',  ( 34.99999999999958789, 1.228057239789091624E-13, -47.50005079999998969 ) ) ;
#10026 = CARTESIAN_POINT ( 'NONE',  ( 3.930324603630738878, -100.3934781419522011, 6.514713691489384395 ) ) ;
#10027 = ADVANCED_FACE ( 'NONE', ( #985 ), #9402, .F. ) ;
#10028 = CARTESIAN_POINT ( 'NONE',  ( 15.29705854078138749, 17.78624592198638155, 1.840275709580739737E-15 ) ) ;
#10029 = ADVANCED_FACE ( 'NONE', ( #5113 ), #13720, .F. ) ;
#10030 = ORIENTED_EDGE ( 'NONE', *, *, #3431, .F. ) ;
#10031 = EDGE_LOOP ( 'NONE', ( #10907, #11027, #4979, #12990 ) ) ;
#10032 = ADVANCED_FACE ( 'NONE', ( #6244 ), #9474, .T. ) ;
#10033 = ADVANCED_FACE ( 'NONE', ( #9864 ), #7749, .T. ) ;
#10034 = CARTESIAN_POINT ( 'NONE',  ( 89.49979561504950709, -156.1132911148542917, -2.500000000000000000 ) ) ;
#10035 = AXIS2_PLACEMENT_3D ( 'NONE', #13305, #3581, #11303 ) ;
#10036 = CARTESIAN_POINT ( 'NONE',  ( 9.601587402597818510, -70.78787878788214982, 2.975959431766512342 ) ) ;
#10037 = EDGE_LOOP ( 'NONE', ( #557, #107, #12420, #11698 ) ) ;
#10038 = CARTESIAN_POINT ( 'NONE',  ( 4.363680981163678751, 91.46147893603955481, 2.443653808501017544 ) ) ;
#10039 =( NAMED_UNIT ( * ) SI_UNIT ( $, .STERADIAN. ) SOLID_ANGLE_UNIT ( ) );
#10040 = CIRCLE ( 'NONE', #7561, 9.000000000009000800 ) ;
#10041 = DIRECTION ( 'NONE',  ( 6.158143864569485777E-17, 2.736152283717910599E-16, -1.000000000000000000 ) ) ;
#10042 = CARTESIAN_POINT ( 'NONE',  ( 15.29705854078139637, 90.00000000000000000, 1.714422261702873555E-15 ) ) ;
#10043 = LINE ( 'NONE', #592, #435 ) ;
#10044 = CARTESIAN_POINT ( 'NONE',  ( -15.29705854078139460, -18.02629830864593785, -3.728963417185749694E-15 ) ) ;
#10045 = CARTESIAN_POINT ( 'NONE',  ( 3.692320488640516096, -128.7272727272744248, -2.755591346289505417 ) ) ;
#10046 = CARTESIAN_POINT ( 'NONE',  ( 34.99999999999958789, 1.091249486606660213E-13, 2.500000000000000000 ) ) ;
#10047 = EDGE_CURVE ( 'NONE', #11768, #11046, #990, .T. ) ;
#10048 = CARTESIAN_POINT ( 'NONE',  ( 15.61050411040038099, -16.56206589787452188, 1.710375830838840816 ) ) ;
#10049 = ORIENTED_EDGE ( 'NONE', *, *, #10607, .T. ) ;
#10050 = ORIENTED_EDGE ( 'NONE', *, *, #7773, .T. ) ;
#10051 = AXIS2_PLACEMENT_3D ( 'NONE', #11983, #3357, #9891 ) ;
#10052 = CARTESIAN_POINT ( 'NONE',  ( -35.00000000000000000, -4.286263797015736496E-15, -7.500000000000000000 ) ) ;
#10053 = EDGE_LOOP ( 'NONE', ( #1726, #9141, #6153, #1660, #12198, #9160 ) ) ;
#10054 = EDGE_CURVE ( 'NONE', #9032, #1176, #4407, .T. ) ;
#10055 = AXIS2_PLACEMENT_3D ( 'NONE', #3500, #12071, #9904 ) ;
#10056 = ADVANCED_FACE ( 'NONE', ( #1374 ), #6635, .T. ) ;
#10057 = CARTESIAN_POINT ( 'NONE',  ( 1.528183159915511125, -102.9021681410130356, -7.139114381135374998 ) ) ;
#10058 = CARTESIAN_POINT ( 'NONE',  ( 39.71817523509052705, -20.60992048131556942, -2.500000000000004441 ) ) ;
#10059 = DIRECTION ( 'NONE',  ( 0.4545454545454531425, 0.8907235428302472391, 0.000000000000000000 ) ) ;
#10060 = CARTESIAN_POINT ( 'NONE',  ( -0.1215172727492840610, -143.6254824914774701, 2.565777989091288180 ) ) ;
#10061 = CIRCLE ( 'NONE', #3781, 5.000000000000005329 ) ;
#10062 = DIRECTION ( 'NONE',  ( -2.797435172181481150E-17, 1.000000000000000000, -1.765856845898762549E-18 ) ) ;
#10063 = PLANE ( 'NONE',  #3337 ) ;
#10064 = DIRECTION ( 'NONE',  ( 1.000000000000000000, 0.000000000000000000, -0.000000000000000000 ) ) ;
#10065 = APPLICATION_CONTEXT ( 'automotive_design' ) ;
#10066 = EDGE_CURVE ( 'NONE', #2729, #11081, #3617, .T. ) ;
#10067 = DIRECTION ( 'NONE',  ( 2.797435172181480534E-17, -1.000000000000000000, 1.765856845898762164E-18 ) ) ;
#10068 = DIRECTION ( 'NONE',  ( -1.000000000000000000, 0.000000000000000000, 0.000000000000000000 ) ) ;
#10069 = DIRECTION ( 'NONE',  ( -2.797435172181481150E-17, 1.000000000000000000, -1.765856845898762549E-18 ) ) ;
#10070 = DIRECTION ( 'NONE',  ( -6.158143864569485777E-17, -2.736152283717910599E-16, 1.000000000000000000 ) ) ;
#10071 = ADVANCED_FACE ( 'NONE', ( #11049 ), #419, .F. ) ;
#10072 = ORIENTED_EDGE ( 'NONE', *, *, #7706, .T. ) ;
#10073 = LINE ( 'NONE', #6909, #12078 ) ;
#10074 = CIRCLE ( 'NONE', #2435, 5.000000000000000888 ) ;
#10075 = ORIENTED_EDGE ( 'NONE', *, *, #13592, .F. ) ;
#10076 = CARTESIAN_POINT ( 'NONE',  ( -3.056920711451915018, -140.5584415584246187, -3.800163123440760238 ) ) ;
#10077 = CIRCLE ( 'NONE', #1559, 2.000000000000000000 ) ;
#10078 = VERTEX_POINT ( 'NONE', #8732 ) ;
#10079 = CARTESIAN_POINT ( 'NONE',  ( 17.19653809941365452, 5.878923826270381348, -2.499999999999999112 ) ) ;
#10080 = APPLICATION_PROTOCOL_DEFINITION ( 'draft international standard', 'automotive_design', 1998, #4587 ) ;
#10081 = ORIENTED_EDGE ( 'NONE', *, *, #13335, .F. ) ;
#10082 = CARTESIAN_POINT ( 'NONE',  ( -56.97938482099326762, -167.3636363668308888, -8.923382220094675077 ) ) ;
#10083 = CIRCLE ( 'NONE', #4925, 25.50000000002550138 ) ;
#10084 = CYLINDRICAL_SURFACE ( 'NONE', #8973, 9.000000000008999024 ) ;
#10085 = CARTESIAN_POINT ( 'NONE',  ( -39.10224891377573897, 101.4936815461678208, 2.486392430613896032 ) ) ;
#10086 = AXIS2_PLACEMENT_3D ( 'NONE', #2394, #317, #4571 ) ;
#10087 = CARTESIAN_POINT ( 'NONE',  ( 26.79177319725820539, -26.24642857144861807, -4.000000000000000000 ) ) ;
#10088 = CIRCLE ( 'NONE', #8505, 15.29705854078138927 ) ;
#10089 = CARTESIAN_POINT ( 'NONE',  ( -15.29705854078138927, -38.76242177807012723, 6.844888786042043893E-17 ) ) ;
#10090 = VERTEX_POINT ( 'NONE', #7423 ) ;
#10091 = B_SPLINE_CURVE_WITH_KNOTS ( 'NONE', 3,
 ( #3048, #5283, #4023, #8310 ),
 .UNSPECIFIED., .F., .F.,
 ( 4, 4 ),
 ( 0.000000000000000000, 1.000000000000000000 ),
 .UNSPECIFIED. ) ;
#10092 = DIRECTION ( 'NONE',  ( -0.9960067511297463483, 0.08927794634716618161, -4.818676322152979407E-17 ) ) ;
#10093 = AXIS2_PLACEMENT_3D ( 'NONE', #2278, #1235, #12023 ) ;
#10094 = CIRCLE ( 'NONE', #2029, 9.000000000009000800 ) ;
#10095 = ORIENTED_EDGE ( 'NONE', *, *, #7285, .F. ) ;
#10096 = VERTEX_POINT ( 'NONE', #2574 ) ;
#10097 = CARTESIAN_POINT ( 'NONE',  ( 10.69346802281035202, -35.22415542633469698, -21.38693604562068984 ) ) ;
#10098 = DIRECTION ( 'NONE',  ( -1.000000000000000000, 0.000000000000000000, 0.000000000000000000 ) ) ;
#10099 = CARTESIAN_POINT ( 'NONE',  ( -12.99579180576516713, 35.80917582696438473, -1.717993240291646161E-15 ) ) ;
#10100 = DIRECTION ( 'NONE',  ( -0.000000000000000000, -0.000000000000000000, 1.000000000000000000 ) ) ;
#10101 = CARTESIAN_POINT ( 'NONE',  ( 5.563246471219282618, -98.57715322402732738, 5.512450067888273075 ) ) ;
#10102 = VECTOR ( 'NONE', #10001, 1000.000000000000000 ) ;
#10103 = CARTESIAN_POINT ( 'NONE',  ( 8.385254915620286909, 59.82872437272870769, 16.77050983124058448 ) ) ;
#10104 = ORIENTED_EDGE ( 'NONE', *, *, #90, .T. ) ;
#10105 = AXIS2_PLACEMENT_3D ( 'NONE', #217, #11976, #12 ) ;
#10106 = CIRCLE ( 'NONE', #4053, 8.385254915620290461 ) ;
#10107 = ORIENTED_EDGE ( 'NONE', *, *, #2935, .F. ) ;
#10108 = VERTEX_POINT ( 'NONE', #5801 ) ;
#10109 = ORIENTED_EDGE ( 'NONE', *, *, #8641, .F. ) ;
#10110 = EDGE_CURVE ( 'NONE', #4633, #11396, #267, .T. ) ;
#10111 = DIRECTION ( 'NONE',  ( 1.000000000000000000, 0.000000000000000000, 0.000000000000000000 ) ) ;
#10112 = CARTESIAN_POINT ( 'NONE',  ( 9.888538082662813977, -70.78787878787576915, 1.806551902650904484 ) ) ;
#10113 = EDGE_LOOP ( 'NONE', ( #3245, #1455, #682, #439 ) ) ;
#10114 = CARTESIAN_POINT ( 'NONE',  ( 5.938565219940902473, -74.76276777339397484, 8.199189651718064908 ) ) ;
#10115 = CIRCLE ( 'NONE', #7421, 16.99999999999998934 ) ;
#10116 = FACE_OUTER_BOUND ( 'NONE', #1222, .T. ) ;
#10117 = PLANE ( 'NONE',  #9388 ) ;
#10118 = CARTESIAN_POINT ( 'NONE',  ( 12.99553232110415024, -17.19957910547634228, -25.99106464220828627 ) ) ;
#10119 = CARTESIAN_POINT ( 'NONE',  ( -3.341303593452078058, -106.9090909090913755, 6.231874970755803211 ) ) ;
#10120 = CYLINDRICAL_SURFACE ( 'NONE', #13600, 15.29705854078139105 ) ;
#10121 = FACE_OUTER_BOUND ( 'NONE', #10113, .T. ) ;
#10122 = DIRECTION ( 'NONE',  ( -1.000000000000000000, -1.224646799147353207E-16, 0.000000000000000000 ) ) ;
#10123 = ORIENTED_EDGE ( 'NONE', *, *, #816, .T. ) ;
#10124 = ORIENTED_EDGE ( 'NONE', *, *, #9696, .F. ) ;
#10125 = DIRECTION ( 'NONE',  ( 1.000000000000000000, 0.000000000000000000, 0.000000000000000000 ) ) ;
#10126 = ORIENTED_EDGE ( 'NONE', *, *, #13221, .F. ) ;
#10127 = STYLED_ITEM ( 'NONE', ( #3549 ), #3056 ) ;
#10128 = CARTESIAN_POINT ( 'NONE',  ( 6.160012261085373808, -112.2768544234564416, -0.06296530155695967412 ) ) ;
#10129 = LINE ( 'NONE', #5997, #13235 ) ;
#10130 = EDGE_CURVE ( 'NONE', #1977, #4304, #2325, .T. ) ;
#10131 = CARTESIAN_POINT ( 'NONE',  ( -35.00000000000000000, -4.286263797015736496E-15, -8.499999999999998224 ) ) ;
#10132 = ORIENTED_EDGE ( 'NONE', *, *, #3242, .F. ) ;
#10133 = ORIENTED_EDGE ( 'NONE', *, *, #43, .T. ) ;
#10134 = DIRECTION ( 'NONE',  ( 1.000000000000000000, -3.851859888774468203E-30, 1.387778780781445676E-15 ) ) ;
#10135 = VERTEX_POINT ( 'NONE', #5725 ) ;
#10136 = EDGE_CURVE ( 'NONE', #1146, #8762, #1675, .T. ) ;
#10137 = CARTESIAN_POINT ( 'NONE',  ( 2.898805451609365758, -136.7680419189706811, 1.590792564838447998 ) ) ;
#10138 = CARTESIAN_POINT ( 'NONE',  ( 4.769534092270758308, 90.26591089801031842, -1.504791211541889329 ) ) ;
#10139 = CARTESIAN_POINT ( 'NONE',  ( -2.517691654963332357E-15, 90.00000000000000000, -1.589271161308885878E-16 ) ) ;
#10140 = EDGE_CURVE ( 'NONE', #8984, #470, #2505, .T. ) ;
#10141 = CARTESIAN_POINT ( 'NONE',  ( 9.847276892489302169E-17, -3.520109059331727686, 6.216008680731233110E-18 ) ) ;
#10142 = EDGE_CURVE ( 'NONE', #3010, #1557, #11131, .T. ) ;
#10143 = PRODUCT_DEFINITION_SHAPE ( 'NONE', 'NONE',  #13900 ) ;
#10144 = DIRECTION ( 'NONE',  ( -0.000000000000000000, -0.000000000000000000, -1.000000000000000000 ) ) ;
#10145 = CARTESIAN_POINT ( 'NONE',  ( -15.18222645069203125, -100.0000000000000000, 4.000000000000000000 ) ) ;
#10146 = LINE ( 'NONE', #12174, #9329 ) ;
#10147 = CARTESIAN_POINT ( 'NONE',  ( 15.29705854078139282, -8.601520358636511432, 1.890204135573039875E-15 ) ) ;
#10148 = DIRECTION ( 'NONE',  ( 5.551115123125776539E-17, -1.000000000000000000, -3.944304526105059027E-31 ) ) ;
#10149 = ORIENTED_EDGE ( 'NONE', *, *, #9972, .F. ) ;
#10150 = CARTESIAN_POINT ( 'NONE',  ( -12.93801431150469128, -134.6363636363606986, 1.977757875721223968 ) ) ;
#10151 = AXIS2_PLACEMENT_3D ( 'NONE', #6562, #9652, #3194 ) ;
#10152 = ADVANCED_FACE ( 'NONE', ( #4675 ), #6378, .T. ) ;
#10153 = EDGE_LOOP ( 'NONE', ( #5700, #12395, #5547, #5780 ) ) ;
#10154 = DIRECTION ( 'NONE',  ( 0.000000000000000000, 0.000000000000000000, 1.000000000000000000 ) ) ;
#10155 = LINE ( 'NONE', #11400, #10189 ) ;
#10156 = CARTESIAN_POINT ( 'NONE',  ( 10.69381717166375445, 34.98422482212468054, 1.263224666758019907E-15 ) ) ;
#10157 = ADVANCED_FACE ( 'NONE', ( #9936 ), #11731, .T. ) ;
#10158 = LINE ( 'NONE', #1736, #10536 ) ;
#10159 = CARTESIAN_POINT ( 'NONE',  ( -31.93204061526059334, -135.0000000000000000, 0.000000000000000000 ) ) ;
#10160 = DIRECTION ( 'NONE',  ( 0.6000000000000006439, -0.7999999999999996003, 0.000000000000000000 ) ) ;
#10161 = CARTESIAN_POINT ( 'NONE',  ( -12.97449437267217576, -39.59556244224027211, -1.449077110393148750E-15 ) ) ;
#10162 = DIRECTION ( 'NONE',  ( 0.9960067511297463483, -0.08927794634716620936, 4.626175998653454121E-17 ) ) ;
#10163 = ORIENTED_EDGE ( 'NONE', *, *, #9718, .T. ) ;
#10164 = ORIENTED_EDGE ( 'NONE', *, *, #6097, .T. ) ;
#10165 = CARTESIAN_POINT ( 'NONE',  ( 8.385254915620294014, 31.55439052270045508, 9.688596779957294507E-16 ) ) ;
#10166 = ORIENTED_EDGE ( 'NONE', *, *, #7138, .F. ) ;
#10167 = ORIENTED_EDGE ( 'NONE', *, *, #1652, .F. ) ;
#10168 = FILL_AREA_STYLE_COLOUR ( '', #9438 ) ;
#10169 = AXIS2_PLACEMENT_3D ( 'NONE', #9565, #1783, #13677 ) ;
#10170 = CARTESIAN_POINT ( 'NONE',  ( 19.51309799441515835, 26.83545189264578212, 4.432601239563248363 ) ) ;
#10171 = DIRECTION ( 'NONE',  ( -6.158143864569485777E-17, -2.736152283717910599E-16, 1.000000000000000000 ) ) ;
#10172 = CARTESIAN_POINT ( 'NONE',  ( 1.383078971141448177, -102.9954216821132746, 7.191944656388454149 ) ) ;
#10173 = CARTESIAN_POINT ( 'NONE',  ( -8.385254915620297567, 50.40394642271930792, -2.186308893455868305E-15 ) ) ;
#10174 = ORIENTED_EDGE ( 'NONE', *, *, #7196, .T. ) ;
#10175 = ORIENTED_EDGE ( 'NONE', *, *, #5565, .T. ) ;
#10176 = AXIS2_PLACEMENT_3D ( 'NONE', #12033, #4520, #10973 ) ;
#10177 = VERTEX_POINT ( 'NONE', #2422 ) ;
#10178 = CARTESIAN_POINT ( 'NONE',  ( -9.736331930512843513, -69.99978782402621391, -2.722951059031194276 ) ) ;
#10179 = CARTESIAN_POINT ( 'NONE',  ( 8.599520226296911929, -74.45454545454452955, 5.474475378420848415 ) ) ;
#10180 = ORIENTED_EDGE ( 'NONE', *, *, #2211, .T. ) ;
#10181 = CARTESIAN_POINT ( 'NONE',  ( 4.942677383991346041, 90.01345119373434045, 0.7661926690451046351 ) ) ;
#10182 = LINE ( 'NONE', #727, #3322 ) ;
#10183 = CARTESIAN_POINT ( 'NONE',  ( 35.00000000000000711, -25.00000000000000000, 7.500000000000000000 ) ) ;
#10184 = CARTESIAN_POINT ( 'NONE',  ( -5.390560935658909258, -117.0909090909071750, -3.329211565280856266 ) ) ;
#10185 = CARTESIAN_POINT ( 'NONE',  ( -39.06230589874905235, 109.5835921350012825, -2.499999999999999556 ) ) ;
#10186 = CIRCLE ( 'NONE', #9698, 71.99999999999998579 ) ;
#10187 = FACE_OUTER_BOUND ( 'NONE', #4406, .T. ) ;
#10188 = CARTESIAN_POINT ( 'NONE',  ( -8.385254915620292238, 43.60378069071538221, -7.699803463976802609E-17 ) ) ;
#10189 = VECTOR ( 'NONE', #13417, 1000.000000000000000 ) ;
#10190 = VERTEX_POINT ( 'NONE', #5650 ) ;
#10191 = ORIENTED_EDGE ( 'NONE', *, *, #5847, .T. ) ;
#10192 = VERTEX_POINT ( 'NONE', #4599 ) ;
#10193 = CARTESIAN_POINT ( 'NONE',  ( 0.2490282479001026672, -158.6998983971402026, 1.476456505561915877 ) ) ;
#10194 = AXIS2_PLACEMENT_3D ( 'NONE', #10202, #7108, #11382 ) ;
#10195 = ORIENTED_EDGE ( 'NONE', *, *, #13612, .F. ) ;
#10196 = CARTESIAN_POINT ( 'NONE',  ( -3.658761532827469409, -133.3911832492017595, 0.09517750528092941420 ) ) ;
#10197 = CARTESIAN_POINT ( 'NONE',  ( 52.27091746333575628, 18.76074118940758240, -2.499999999999992895 ) ) ;
#10198 = CARTESIAN_POINT ( 'NONE',  ( 57.84299132690245671, 11.33347904398043049, -2.499999999999994671 ) ) ;
#10199 = CARTESIAN_POINT ( 'NONE',  ( 22.31663499682298735, 16.91633092580596198, 2.500000000000003997 ) ) ;
#10200 = ORIENTED_EDGE ( 'NONE', *, *, #11155, .T. ) ;
#10201 = ORIENTED_EDGE ( 'NONE', *, *, #10970, .F. ) ;
#10202 = CARTESIAN_POINT ( 'NONE',  ( -1.288514859053046853E-15, 46.06057977201469100, -8.133639011647813827E-17 ) ) ;
#10203 = CARTESIAN_POINT ( 'NONE',  ( 0.3257135472934549747, -142.6406298964565451, 2.652232148860325101 ) ) ;
#10204 = CARTESIAN_POINT ( 'NONE',  ( 14.13596196814457606, -39.17949320881311337, 0.000000000000000000 ) ) ;
#10205 = COLOUR_RGB ( '', 0.40784314, 0.44705882, 0.49803922) ;
#10206 = DIRECTION ( 'NONE',  ( 1.000000000000000000, 0.000000000000000000, 0.000000000000000000 ) ) ;
#10207 = CARTESIAN_POINT ( 'NONE',  ( 0.000000000000000000, 71.01020514433645303, -0.5000000000000000000 ) ) ;
#10208 = CARTESIAN_POINT ( 'NONE',  ( 0.000000000000000000, 20.00000000000000355, 0.000000000000000000 ) ) ;
#10209 = FACE_OUTER_BOUND ( 'NONE', #4612, .T. ) ;
#10210 = EDGE_CURVE ( 'NONE', #6099, #10920, #5242, .T. ) ;
#10211 = EDGE_CURVE ( 'NONE', #2392, #8894, #5683, .T. ) ;
#10212 = AXIS2_PLACEMENT_3D ( 'NONE', #7025, #8926, #6747 ) ;
#10213 = EDGE_CURVE ( 'NONE', #2480, #4529, #936, .T. ) ;
#10214 = VERTEX_POINT ( 'NONE', #3690 ) ;
#10215 = CARTESIAN_POINT ( 'NONE',  ( -8.385254915620288685, 53.02855864072483882, -16.77050983124058092 ) ) ;
#10216 = PRODUCT_DEFINITION_FORMATION_WITH_SPECIFIED_SOURCE ( 'ANY', '', #13292, .NOT_KNOWN. ) ;
#10217 = CARTESIAN_POINT ( 'NONE',  ( 14.14432607165388056, -111.7272727272740838, -3.395498375151920101 ) ) ;
#10218 = ADVANCED_FACE ( 'NONE', ( #2644 ), #6156, .F. ) ;
#10219 = EDGE_CURVE ( 'NONE', #131, #12059, #1434, .T. ) ;
#10220 = ORIENTED_EDGE ( 'NONE', *, *, #10567, .F. ) ;
#10221 = ORIENTED_EDGE ( 'NONE', *, *, #8327, .F. ) ;
#10222 = CARTESIAN_POINT ( 'NONE',  ( -4.658052367537133698, 90.49197326372723182, -1.819943918220761514 ) ) ;
#10223 = DIRECTION ( 'NONE',  ( 1.000000000000000000, 0.000000000000000000, 0.000000000000000000 ) ) ;
#10224 = CARTESIAN_POINT ( 'NONE',  ( 2.139171521560111700, -164.3636363655099615, 0.7092570206224070306 ) ) ;
#10225 = DIRECTION ( 'NONE',  ( -1.000000000000000000, 0.000000000000000000, 0.000000000000000000 ) ) ;
#10226 = LINE ( 'NONE', #8049, #7232 ) ;
#10227 = PRODUCT_DEFINITION_CONTEXT ( 'detailed design', #10837, 'design' ) ;
#10228 = CARTESIAN_POINT ( 'NONE',  ( 10.09953664735706447, -70.24026703789812132, 0.01926284265930006817 ) ) ;
#10229 = ADVANCED_FACE ( 'NONE', ( #827 ), #12541, .T. ) ;
#10230 = ORIENTED_EDGE ( 'NONE', *, *, #7122, .T. ) ;
#10231 = ORIENTED_EDGE ( 'NONE', *, *, #13499, .F. ) ;
#10232 = EDGE_CURVE ( 'NONE', #6733, #8612, #9057, .T. ) ;
#10233 = ORIENTED_EDGE ( 'NONE', *, *, #2135, .T. ) ;
#10234 = CARTESIAN_POINT ( 'NONE',  ( -8.385254915620294014, -34.41905512736551032, -16.77050983124059869 ) ) ;
#10235 = AXIS2_PLACEMENT_3D ( 'NONE', #346, #3766, #12406 ) ;
#10236 = FACE_OUTER_BOUND ( 'NONE', #3845, .T. ) ;
#10237 = CARTESIAN_POINT ( 'NONE',  ( 19.99988111993866724, 26.72048013816596779, -0.6453928856983822682 ) ) ;
#10238 = CARTESIAN_POINT ( 'NONE',  ( -34.78790783510986984, 106.9804631782722169, 2.384639261440467006 ) ) ;
#10239 = CARTESIAN_POINT ( 'NONE',  ( -2.835131095452588124, -107.5510716257525843, 6.137765108552229343 ) ) ;
#10240 = CARTESIAN_POINT ( 'NONE',  ( -36.36363636363635976, 142.2680885707561629, -0.5000000000000000000 ) ) ;
#10241 = VERTEX_POINT ( 'NONE', #2922 ) ;
#10242 = ORIENTED_EDGE ( 'NONE', *, *, #2844, .T. ) ;
#10243 = EDGE_CURVE ( 'NONE', #7167, #6716, #4552, .T. ) ;
#10244 = ORIENTED_EDGE ( 'NONE', *, *, #12082, .T. ) ;
#10245 = CARTESIAN_POINT ( 'NONE',  ( -25.00000000000000000, -35.00000000000000000, -7.500000000000000000 ) ) ;
#10246 = CARTESIAN_POINT ( 'NONE',  ( -8.385254915620294014, 90.00000000000000000, -1.589271161308885878E-16 ) ) ;
#10247 = ORIENTED_EDGE ( 'NONE', *, *, #12955, .T. ) ;
#10248 = CARTESIAN_POINT ( 'NONE',  ( 9.515638018240474949, -70.53215315925814366, 3.421011899655237887 ) ) ;
#10249 = SURFACE_STYLE_FILL_AREA ( #2885 ) ;
#10250 = DIRECTION ( 'NONE',  ( 1.000000000000000000, 1.601283208593975514E-16, -0.000000000000000000 ) ) ;
#10251 = CARTESIAN_POINT ( 'NONE',  ( -8.385254915620290461, -15.56949922734665748, -16.77050983124058803 ) ) ;
#10252 = CARTESIAN_POINT ( 'NONE',  ( 0.8583871962662020794, -102.5454545454553568, 7.611802117357260755 ) ) ;
#10253 = CYLINDRICAL_SURFACE ( 'NONE', #3716, 15.70031846811053455 ) ;
#10254 = B_SPLINE_CURVE_WITH_KNOTS ( 'NONE', 3,
 ( #5934, #10204, #8368, #7374 ),
 .UNSPECIFIED., .F., .F.,
 ( 4, 4 ),
 ( 0.000000000000000000, 1.000000000000000000 ),
 .UNSPECIFIED. ) ;
#10255 = CARTESIAN_POINT ( 'NONE',  ( 15.64391473689848233, -16.60099851263468196, 1.372939470208868196 ) ) ;
#10256 = SURFACE_STYLE_USAGE ( .BOTH. , #5768 ) ;
#10257 = ORIENTED_EDGE ( 'NONE', *, *, #9699, .F. ) ;
#10258 = VERTEX_POINT ( 'NONE', #1594 ) ;
#10259 = ORIENTED_EDGE ( 'NONE', *, *, #7336, .T. ) ;
#10260 = EDGE_LOOP ( 'NONE', ( #1385, #3271, #7592, #6364, #3533 ) ) ;
#10261 = CARTESIAN_POINT ( 'NONE',  ( 0.3820449743694532829, -101.7806079922463169, -7.430334148094327240 ) ) ;
#10262 = VECTOR ( 'NONE', #1192, 1000.000000000000000 ) ;
#10263 = B_SPLINE_CURVE_WITH_KNOTS ( 'NONE', 3,
 ( #995, #1065, #10780, #6318, #5259, #5328, #5458, #9744, #4402, #3354, #7635, #11910, #2300, #512, #3484, #2663, #1468, #436 ),
 .UNSPECIFIED., .F., .F.,
 ( 4, 2, 2, 2, 2, 2, 2, 2, 4 ),
 ( 2.478944061727388434E-07, 0.0003651306916264178350, 0.0007300134888466628617, 0.001094896286066908159, 0.001459779083287153023, 0.001824661880507398104, 0.002189544677727643836, 0.002554427474947888917, 0.002919310272168133130 ),
 .UNSPECIFIED. ) ;
#10264 = CARTESIAN_POINT ( 'NONE',  ( -8.385254915620297567, 31.55439052270045508, -5.572053652267360357E-17 ) ) ;
#10265 = CARTESIAN_POINT ( 'NONE',  ( -2.517691654963332357E-15, 90.00000000000000000, -1.589271161308885878E-16 ) ) ;
#10266 = CARTESIAN_POINT ( 'NONE',  ( 25.00000000000000355, 120.0000000000000284, -0.5000000000000000000 ) ) ;
#10267 = CARTESIAN_POINT ( 'NONE',  ( 1.640938733393168425, -125.5689954488632907, -4.287054131913241584 ) ) ;
#10268 = EDGE_CURVE ( 'NONE', #5587, #11738, #10155, .T. ) ;
#10269 = CARTESIAN_POINT ( 'NONE',  ( 4.338055960494658692, 91.73205429892865936, -2.486400748338238653 ) ) ;
#10270 = CARTESIAN_POINT ( 'NONE',  ( -35.00000000000000000, -4.286263797015736496E-15, 7.500000000000000000 ) ) ;
#10271 = CARTESIAN_POINT ( 'NONE',  ( -25.00000000000000355, 120.0000000000000142, -2.499999999999998668 ) ) ;
#10272 = DIRECTION ( 'NONE',  ( 0.000000000000000000, -1.000000000000000000, 0.000000000000000000 ) ) ;
#10273 = AXIS2_PLACEMENT_3D ( 'NONE', #9801, #10642, #208 ) ;
#10274 = FACE_OUTER_BOUND ( 'NONE', #7934, .T. ) ;
#10275 = CARTESIAN_POINT ( 'NONE',  ( 0.000000000000000000, 71.01020514433645303, 2.499999999999999556 ) ) ;
#10276 = CARTESIAN_POINT ( 'NONE',  ( 12.99579180576516180, 64.08350967699263379, 25.99158361153034136 ) ) ;
#10277 = AXIS2_PLACEMENT_3D ( 'NONE', #2385, #171, #234 ) ;
#10278 = VERTEX_POINT ( 'NONE', #1734 ) ;
#10279 = CARTESIAN_POINT ( 'NONE',  ( 8.385254915620290461, 53.02855864072483882, -16.77050983124057737 ) ) ;
#10280 = ORIENTED_EDGE ( 'NONE', *, *, #9614, .T. ) ;
#10281 = CARTESIAN_POINT ( 'NONE',  ( 3.682460330391462033, -161.0909090907768189, 2.758257593130142737 ) ) ;
#10282 = ORIENTED_EDGE ( 'NONE', *, *, #8834, .F. ) ;
#10283 = CIRCLE ( 'NONE', #12061, 77.99999999999997158 ) ;
#10284 = ORIENTED_EDGE ( 'NONE', *, *, #10213, .T. ) ;
#10285 = CARTESIAN_POINT ( 'NONE',  ( -4.696484759529494291, 90.40938722714874132, -1.719265504264336109 ) ) ;
#10286 = CARTESIAN_POINT ( 'NONE',  ( -15.34998809918498353, -16.25417180422370933, 3.363251165709652213 ) ) ;
#10287 = EDGE_CURVE ( 'NONE', #2229, #13867, #4128, .T. ) ;
#10288 = CLOSED_SHELL ( 'NONE', ( #11679, #4342, #13060, #7958, #7491, #6510, #10071, #9110, #9418, #11508, #1992, #12170, #2142, #2156, #4294, #13371, #6021, #10309, #1482, #12614, #2865, #12529, #646, #12801, #11411, #4886, #6203, #13353, #10056, #3090, #12187, #6451, #1585, #9471, #11413, #6057, #5240, #6967, #2930, #8528, #11238, #6769, #9357, #9216, #7743, #11174, #7043, #197, #8659, #88, #3959, #1384, #4905, #4669, #6420, #13777, #10731, #12090, #12080, #3961, #2377, #4025, #11033, #6370, #11585, #7308 ) ) ;
#10289 = EDGE_CURVE ( 'NONE', #13160, #3229, #3763, .T. ) ;
#10290 = DIRECTION ( 'NONE',  ( -1.000000000000000000, 0.000000000000000000, 0.000000000000000000 ) ) ;
#10291 = CYLINDRICAL_SURFACE ( 'NONE', #8211, 25.50000000002549783 ) ;
#10292 = ADVANCED_FACE ( 'NONE', ( #12328 ), #9307, .T. ) ;
#10293 = CARTESIAN_POINT ( 'NONE',  ( 51.25836974494252019, 19.64472991003004054, -2.499999999999992450 ) ) ;
#10294 = CIRCLE ( 'NONE', #454, 3.999999999999996447 ) ;
#10295 = DIRECTION ( 'NONE',  ( 0.000000000000000000, 0.000000000000000000, -1.000000000000000000 ) ) ;
#10296 = EDGE_LOOP ( 'NONE', ( #9491, #10259, #10767, #6649 ) ) ;
#10297 = VECTOR ( 'NONE', #10807, 1000.000000000000000 ) ;
#10298 = ORIENTED_EDGE ( 'NONE', *, *, #6602, .T. ) ;
#10299 = CARTESIAN_POINT ( 'NONE',  ( -5.384951958016893414, -83.47453208601771735, 7.985098097371742476 ) ) ;
#10300 = ADVANCED_FACE ( 'NONE', ( #626 ), #6995, .F. ) ;
#10301 = AXIS2_PLACEMENT_3D ( 'NONE', #475, #6901, #5870 ) ;
#10302 = ORIENTED_EDGE ( 'NONE', *, *, #375, .T. ) ;
#10303 = EDGE_CURVE ( 'NONE', #8708, #5686, #2260, .T. ) ;
#10304 = ORIENTED_EDGE ( 'NONE', *, *, #11404, .T. ) ;
#10305 = VECTOR ( 'NONE', #2295, 1000.000000000000000 ) ;
#10306 = FACE_OUTER_BOUND ( 'NONE', #12846, .T. ) ;
#10307 = ADVANCED_FACE ( 'NONE', ( #8184 ), #12468, .T. ) ;
#10308 = CARTESIAN_POINT ( 'NONE',  ( -10.00000000000000000, 99.99999999999994316, -0.5000000000000000000 ) ) ;
#10309 = ADVANCED_FACE ( 'NONE', ( #3973 ), #7394, .T. ) ;
#10310 = PLANE ( 'NONE',  #8423 ) ;
#10311 = CARTESIAN_POINT ( 'NONE',  ( -5.225617147457730205, -118.1447657390923922, -1.522498834799536294 ) ) ;
#10312 = LINE ( 'NONE', #4185, #7340 ) ;
#10313 = CIRCLE ( 'NONE', #900, 4.999999999999998224 ) ;
#10314 = VERTEX_POINT ( 'NONE', #10618 ) ;
#10315 = AXIS2_PLACEMENT_3D ( 'NONE', #2203, #6490, #11883 ) ;
#10316 = VECTOR ( 'NONE', #1569, 1000.000000000000114 ) ;
#10317 = VERTEX_POINT ( 'NONE', #12610 ) ;
#10318 = CARTESIAN_POINT ( 'NONE',  ( -4.231485814931500222, 91.18833760977217651, -2.665113332093635101 ) ) ;
#10319 = CARTESIAN_POINT ( 'NONE',  ( -35.20000000000000995, 106.4000000000000199, 2.500000000000000000 ) ) ;
#10320 = EDGE_LOOP ( 'NONE', ( #10678, #1911, #13279, #6936 ) ) ;
#10321 = CARTESIAN_POINT ( 'NONE',  ( 4.867363524069543423, 90.10434700764739091, 1.150748602993065139 ) ) ;
#10322 =( NAMED_UNIT ( * ) SI_UNIT ( $, .STERADIAN. ) SOLID_ANGLE_UNIT ( ) );
#10323 = VECTOR ( 'NONE', #6985, 1000.000000000000114 ) ;
#10324 = CARTESIAN_POINT ( 'NONE',  ( 12.99579180576516535, 45.23395377697384134, 3.183050967463142591E-15 ) ) ;
#10325 = CARTESIAN_POINT ( 'NONE',  ( -24.99999999999998934, -100.0000000000000000, 7.500000000000000000 ) ) ;
#10326 = ADVANCED_FACE ( 'NONE', ( #11744 ), #889, .T. ) ;
#10327 = CARTESIAN_POINT ( 'NONE',  ( 31.01425004688410070, -18.32044754671509423, 2.499999999999994671 ) ) ;
#10328 = CIRCLE ( 'NONE', #13729, 22.99999999999999645 ) ;
#10329 = DIRECTION ( 'NONE',  ( -0.000000000000000000, -0.000000000000000000, -1.000000000000000000 ) ) ;
#10330 = LINE ( 'NONE', #731, #7974 ) ;
#10331 = ORIENTED_EDGE ( 'NONE', *, *, #4816, .F. ) ;
#10332 = ORIENTED_EDGE ( 'NONE', *, *, #3701, .F. ) ;
#10333 = ORIENTED_EDGE ( 'NONE', *, *, #456, .F. ) ;
#10334 = ORIENTED_EDGE ( 'NONE', *, *, #13335, .T. ) ;
#10335 = CARTESIAN_POINT ( 'NONE',  ( 3.943110440846829157, -117.6640828201278026, 3.845144683265616870 ) ) ;
#10336 = AXIS2_PLACEMENT_3D ( 'NONE', #673, #746, #11189 ) ;
#10337 = AXIS2_PLACEMENT_3D ( 'NONE', #7219, #9334, #916 ) ;
#10338 = CARTESIAN_POINT ( 'NONE',  ( -12.99553232110414314, 29.92431064457076673, -1.697177803646649065E-15 ) ) ;
#10339 = DIRECTION ( 'NONE',  ( -0.000000000000000000, -0.000000000000000000, -1.000000000000000000 ) ) ;
#10340 = ORIENTED_EDGE ( 'NONE', *, *, #6303, .F. ) ;
#10341 = DIRECTION ( 'NONE',  ( 1.000000000000000000, 0.000000000000000000, 0.000000000000000000 ) ) ;
#10342 = CARTESIAN_POINT ( 'NONE',  ( -0.6786374973538379374, -157.4026716423472294, -1.357839624991837413 ) ) ;
#10343 = CARTESIAN_POINT ( 'NONE',  ( 0.1852016367018599341, -70.00000000000000000, -1.488522876466113365 ) ) ;
#10344 = CARTESIAN_POINT ( 'NONE',  ( 2.449293598294706513E-15, 40.00000000000000000, -20.00000000000000000 ) ) ;
#10345 = DIRECTION ( 'NONE',  ( -2.797435172181481150E-17, 1.000000000000000000, -1.765856845898762549E-18 ) ) ;
#10346 = CARTESIAN_POINT ( 'NONE',  ( 31.93204061526061466, -132.0000000000000000, 3.910547132972217398E-15 ) ) ;
#10347 = CARTESIAN_POINT ( 'NONE',  ( -2.517691654963332357E-15, 90.00000000000000000, -1.589271161308885878E-16 ) ) ;
#10348 = CARTESIAN_POINT ( 'NONE',  ( 42.16244658108818300, 105.4500712252157655, -2.499999999999999556 ) ) ;
#10349 = CARTESIAN_POINT ( 'NONE',  ( 10.29982004912477578, -6.336490384724132952, 2.499999999999996447 ) ) ;
#10350 = VERTEX_POINT ( 'NONE', #6224 ) ;
#10351 = CARTESIAN_POINT ( 'NONE',  ( -10.00000000000000711, 139.9999999999999716, 0.5000000000000000000 ) ) ;
#10352 = ORIENTED_EDGE ( 'NONE', *, *, #13161, .T. ) ;
#10353 = CARTESIAN_POINT ( 'NONE',  ( 54.35437857507979231, -62.63636364489408237, 19.28415345520743429 ) ) ;
#10354 = ORIENTED_EDGE ( 'NONE', *, *, #4823, .F. ) ;
#10355 = ORIENTED_EDGE ( 'NONE', *, *, #7990, .F. ) ;
#10356 = CARTESIAN_POINT ( 'NONE',  ( -4.867363524069549641, 90.10434700764739091, -1.150748602993065139 ) ) ;
#10357 = DIRECTION ( 'NONE',  ( 1.000000000000000000, 0.000000000000000000, 0.000000000000000000 ) ) ;
#10358 = CARTESIAN_POINT ( 'NONE',  ( 9.412634226148496097, -71.99999999999992895, 5.970118669234167008 ) ) ;
#10359 = CARTESIAN_POINT ( 'NONE',  ( -11.72298137502696669, -168.9999999999999147, -2.970135970081303256 ) ) ;
#10360 = CARTESIAN_POINT ( 'NONE',  ( 15.29705854078138394, 38.52236939141059935, 1.806990092252540040E-15 ) ) ;
#10361 = LINE ( 'NONE', #9243, #10663 ) ;
#10362 = FACE_OUTER_BOUND ( 'NONE', #12298, .T. ) ;
#10363 = UNCERTAINTY_MEASURE_WITH_UNIT (LENGTH_MEASURE( 1.000000000000000082E-05 ), #3864, 'distance_accuracy_value', 'NONE');
#10364 = DIRECTION ( 'NONE',  ( 2.797435172181480534E-17, -1.000000000000000000, 1.765856845898762164E-18 ) ) ;
#10365 = EDGE_CURVE ( 'NONE', #12788, #11308, #10616, .T. ) ;
#10366 = EDGE_LOOP ( 'NONE', ( #11588, #5726 ) ) ;
#10367 = PLANE ( 'NONE',  #8983 ) ;
#10368 = ORIENTED_EDGE ( 'NONE', *, *, #9886, .F. ) ;
#10369 = CARTESIAN_POINT ( 'NONE',  ( -15.29705854078139282, -19.91286587805129926, -30.59411708156279630 ) ) ;
#10370 = PLANE ( 'NONE',  #76 ) ;
#10371 = CARTESIAN_POINT ( 'NONE',  ( 34.37593967123855521, 107.8393652239837195, 1.644494279733350162 ) ) ;
#10372 = DIRECTION ( 'NONE',  ( 0.5753203450992270263, 0.8179281756455796248, 2.409338161076488717E-16 ) ) ;
#10373 = DIRECTION ( 'NONE',  ( -2.797435172181481150E-17, 1.000000000000000000, -1.765856845898762549E-18 ) ) ;
#10374 = CARTESIAN_POINT ( 'NONE',  ( -2.715682715547387271, -123.3573972935287202, -4.033725032893866747 ) ) ;
#10375 = VECTOR ( 'NONE', #5907, 1000.000000000000000 ) ;
#10376 = DIRECTION ( 'NONE',  ( -2.797435172181481150E-17, 1.000000000000000000, -1.765856845898762549E-18 ) ) ;
#10377 = VERTEX_POINT ( 'NONE', #7260 ) ;
#10378 = ADVANCED_FACE ( 'NONE', ( #12678 ), #578, .T. ) ;
#10379 = ORIENTED_EDGE ( 'NONE', *, *, #8413, .T. ) ;
#10380 = EDGE_CURVE ( 'NONE', #2194, #5379, #1896, .T. ) ;
#10381 = ORIENTED_EDGE ( 'NONE', *, *, #2309, .T. ) ;
#10382 = EDGE_CURVE ( 'NONE', #8229, #10692, #3226, .T. ) ;
#10383 = CARTESIAN_POINT ( 'NONE',  ( -15.29705854078139815, -8.601520358636511432, 30.59411708156277854 ) ) ;
#10384 = ADVANCED_FACE ( 'NONE', ( #13755 ), #9574, .F. ) ;
#10385 = ADVANCED_FACE ( 'NONE', ( #9644 ), #8587, .T. ) ;
#10386 = EDGE_LOOP ( 'NONE', ( #13634, #12654, #6242, #6232 ) ) ;
#10387 = CARTESIAN_POINT ( 'NONE',  ( -3.288118420601238601, 90.13403546913524167, -3.770150660886110838 ) ) ;
#10388 = ORIENTED_EDGE ( 'NONE', *, *, #3318, .F. ) ;
#10389 = CARTESIAN_POINT ( 'NONE',  ( -11.81226048336476353, -40.00941361824966691, -23.62452096672953772 ) ) ;
#10390 = ORIENTED_EDGE ( 'NONE', *, *, #10219, .T. ) ;
#10391 = CYLINDRICAL_SURFACE ( 'NONE', #3417, 9.000000000008999024 ) ;
#10392 = AXIS2_PLACEMENT_3D ( 'NONE', #4357, #4421, #7519 ) ;
#10393 = DIRECTION ( 'NONE',  ( 1.000000000000000000, -0.000000000000000000, -0.000000000000000000 ) ) ;
#10394 = DIRECTION ( 'NONE',  ( 0.000000000000000000, 0.000000000000000000, 1.000000000000000000 ) ) ;
#10395 = DIRECTION ( 'NONE',  ( -0.9960067511297463483, 0.08927794634716618161, -4.818676322152979407E-17 ) ) ;
#10396 = CARTESIAN_POINT ( 'NONE',  ( -1.487915231218352785, -147.9615408504190270, -1.535193590670937969 ) ) ;
#10397 = DIRECTION ( 'NONE',  ( -6.158143864569485777E-17, -2.736152283717910599E-16, 1.000000000000000000 ) ) ;
#10398 = ORIENTED_EDGE ( 'NONE', *, *, #368, .T. ) ;
#10399 = ORIENTED_EDGE ( 'NONE', *, *, #12957, .F. ) ;
#10400 = ORIENTED_EDGE ( 'NONE', *, *, #2150, .F. ) ;
#10401 = B_SPLINE_CURVE_WITH_KNOTS ( 'NONE', 3,
 ( #9514, #3123, #2932, #3978 ),
 .UNSPECIFIED., .F., .F.,
 ( 4, 4 ),
 ( 0.000000000000000000, 1.000000000000000000 ),
 .UNSPECIFIED. ) ;
#10402 = DIRECTION ( 'NONE',  ( -2.797435172181481150E-17, 1.000000000000000000, -1.765856845898762549E-18 ) ) ;
#10403 = ADVANCED_FACE ( 'NONE', ( #12890 ), #1028, .T. ) ;
#10404 = DIRECTION ( 'NONE',  ( -2.797435172181481150E-17, 1.000000000000000000, -1.765856845898762549E-18 ) ) ;
#10405 = DIRECTION ( 'NONE',  ( 0.000000000000000000, 0.000000000000000000, 1.000000000000000000 ) ) ;
#10406 = CARTESIAN_POINT ( 'NONE',  ( -5.389985679975356270, -107.9165190526823039, 3.974935440706736323 ) ) ;
#10407 = VECTOR ( 'NONE', #1450, 1000.000000000000000 ) ;
#10408 = CARTESIAN_POINT ( 'NONE',  ( 0.3668613529500256987, -160.9696969691409549, -1.703459722499988338 ) ) ;
#10409 = DIRECTION ( 'NONE',  ( -2.797435172181481150E-17, 1.000000000000000000, -1.765856845898762549E-18 ) ) ;
#10410 = CARTESIAN_POINT ( 'NONE',  ( 10.69346802281034670, 21.32451227372186864, -21.38693604562068273 ) ) ;
#10411 = CARTESIAN_POINT ( 'NONE',  ( 3.621248221984613947E-16, -12.94488700934118341, 2.285881734483108495E-17 ) ) ;
#10412 = CARTESIAN_POINT ( 'NONE',  ( 34.99999999999958789, 1.104930248025249758E-13, -2.499999999999999112 ) ) ;
#10413 = VECTOR ( 'NONE', #1263, 1000.000000000000000 ) ;
#10414 = CARTESIAN_POINT ( 'NONE',  ( 0.000000000000000000, 71.01020514433645303, 0.5000000000000000000 ) ) ;
#10415 = ORIENTED_EDGE ( 'NONE', *, *, #5233, .T. ) ;
#10416 = CARTESIAN_POINT ( 'NONE',  ( -25.00000000000000355, 120.0000000000000142, -0.5000000000000000000 ) ) ;
#10417 = CARTESIAN_POINT ( 'NONE',  ( 3.036220672062631021, -100.2727272727342580, 3.474096187148000503 ) ) ;
#10418 = CIRCLE ( 'NONE', #6170, 17.49999999999999289 ) ;
#10419 = EDGE_CURVE ( 'NONE', #425, #1659, #2571, .T. ) ;
#10420 = ORIENTED_EDGE ( 'NONE', *, *, #12452, .T. ) ;
#10421 = DIRECTION ( 'NONE',  ( -1.000000000000000000, 0.000000000000000000, 0.000000000000000000 ) ) ;
#10422 = ORIENTED_EDGE ( 'NONE', *, *, #3858, .F. ) ;
#10423 = DIRECTION ( 'NONE',  ( 9.860761315262647568E-32, 3.204747427460360459E-31, -1.000000000000000000 ) ) ;
#10424 = CARTESIAN_POINT ( 'NONE',  ( -15.61050411040038099, -16.56206589787452188, -1.710375830838840816 ) ) ;
#10425 = DIRECTION ( 'NONE',  ( -6.158143864569485777E-17, -2.736152283717910599E-16, 1.000000000000000000 ) ) ;
#10426 =( BOUNDED_SURFACE ( )  B_SPLINE_SURFACE ( 3, 3, ( 
 ( #2137, #9787, #7533, #5427 ),
 ( #2341, #1172, #10755, #10687 ),
 ( #8656, #7671, #7400, #11682 ),
 ( #1099, #5358, #57, #4310 ) ),
 .UNSPECIFIED., .F., .F., .F. ) 
 B_SPLINE_SURFACE_WITH_KNOTS ( ( 4, 4 ),
 ( 4, 4 ),
 ( 0.000000000000000000, 1.000000000000000000 ),
 ( 0.000000000000000000, 1.000000000000000000 ),
 .UNSPECIFIED. ) 
 GEOMETRIC_REPRESENTATION_ITEM ( )  RATIONAL_B_SPLINE_SURFACE ( (
 ( 1.000000000000000000, 0.3333333333333334259, 0.3333333333333334259, 1.000000000000000000),
 ( 1.000000000000000000, 0.3333333333333334259, 0.3333333333333334259, 1.000000000000000000),
 ( 1.000000000000000000, 0.3333333333333334259, 0.3333333333333334259, 1.000000000000000000),
 ( 1.000000000000000000, 0.3333333333333334259, 0.3333333333333334259, 1.000000000000000000) ) ) 
 REPRESENTATION_ITEM ( '' )  SURFACE ( )  );
#10427 = CARTESIAN_POINT ( 'NONE',  ( 4.154595973944849696, -168.9999999999999432, -0.9946518452610428884 ) ) ;
#10428 = DIRECTION ( 'NONE',  ( 0.000000000000000000, 0.000000000000000000, 1.000000000000000000 ) ) ;
#10429 = CIRCLE ( 'NONE', #13826, 15.29705854078138749 ) ;
#10430 = DIRECTION ( 'NONE',  ( 2.797435172181479917E-17, -1.000000000000000000, 1.765856845898779112E-18 ) ) ;
#10431 = CARTESIAN_POINT ( 'NONE',  ( 12.97449437267217753, -39.59556244224027211, 3.177834600809665306E-15 ) ) ;
#10432 = MECHANICAL_DESIGN_GEOMETRIC_PRESENTATION_REPRESENTATION (  '', ( #3700 ), #4147 ) ;
#10433 = TOROIDAL_SURFACE ( 'NONE', #1691, 3.999999999999998224, 2.000000000000000000 ) ;
#10434 = EDGE_LOOP ( 'NONE', ( #3397, #5255, #8239, #9420, #3829, #3164, #6618, #202 ) ) ;
#10435 = CARTESIAN_POINT ( 'NONE',  ( -7.925252723941369482, -86.41510259838975117, 5.018155542691334681 ) ) ;
#10436 = AXIS2_PLACEMENT_3D ( 'NONE', #7698, #2368, #1319 ) ;
#10437 = ORIENTED_EDGE ( 'NONE', *, *, #2791, .F. ) ;
#10438 = FACE_OUTER_BOUND ( 'NONE', #4177, .T. ) ;
#10439 = AXIS2_PLACEMENT_3D ( 'NONE', #7180, #13542, #13674 ) ;
#10440 = ADVANCED_FACE ( 'NONE', ( #960 ), #5355, .T. ) ;
#10441 = CARTESIAN_POINT ( 'NONE',  ( 12.99553232110414136, 29.92431064457076673, 1.549257345293556973E-15 ) ) ;
#10442 = CARTESIAN_POINT ( 'NONE',  ( 15.18222645069203125, -100.0000000000000000, 4.000000000000000000 ) ) ;
#10443 = CARTESIAN_POINT ( 'NONE',  ( 0.3898256620743995593, -154.2032979590117918, 1.618808203873735030 ) ) ;
#10444 = CARTESIAN_POINT ( 'NONE',  ( 12.99553232110414314, 48.77386654458962312, -25.99106464220827561 ) ) ;
#10445 = AXIS2_PLACEMENT_3D ( 'NONE', #333, #13030, #8873 ) ;
#10446 = ORIENTED_EDGE ( 'NONE', *, *, #12356, .F. ) ;
#10447 = EDGE_LOOP ( 'NONE', ( #6616, #3426, #570, #8471, #13426, #6750, #10302 ) ) ;
#10448 = ORIENTED_EDGE ( 'NONE', *, *, #6337, .F. ) ;
#10449 = DIRECTION ( 'NONE',  ( -0.000000000000000000, -0.000000000000000000, -1.000000000000000000 ) ) ;
#10450 = AXIS2_PLACEMENT_3D ( 'NONE', #1737, #7265, #4043 ) ;
#10451 = ORIENTED_EDGE ( 'NONE', *, *, #4923, .F. ) ;
#10452 = CARTESIAN_POINT ( 'NONE',  ( -8.385254915620295790, 78.67828027274755698, -16.77050983124059513 ) ) ;
#10453 = VERTEX_POINT ( 'NONE', #7326 ) ;
#10454 = CARTESIAN_POINT ( 'NONE',  ( 25.00000000000000355, 120.0000000000000284, 2.500000000000000000 ) ) ;
#10455 = EDGE_CURVE ( 'NONE', #4214, #8450, #4234, .T. ) ;
#10456 = CARTESIAN_POINT ( 'NONE',  ( -9.841394828007315354, -91.60173160170883477, -2.396245945941702704 ) ) ;
#10457 = DIRECTION ( 'NONE',  ( -0.9462100554738961389, -0.3235529800822217195, -1.387852799596036113E-16 ) ) ;
#10458 = EDGE_CURVE ( 'NONE', #4633, #2958, #7269, .T. ) ;
#10459 = CARTESIAN_POINT ( 'NONE',  ( -14.85082311557358103, -22.21562007816737960, 5.135570635274604889 ) ) ;
#10460 = DIRECTION ( 'NONE',  ( 2.797435172181480534E-17, -1.000000000000000000, 1.765856845898762164E-18 ) ) ;
#10461 = CARTESIAN_POINT ( 'NONE',  ( -2.440375224551862843, -143.3570535663918122, -0.8181369023438933574 ) ) ;
#10462 = CARTESIAN_POINT ( 'NONE',  ( 15.29705854078138749, 17.78624592198638155, 1.840275709580739737E-15 ) ) ;
#10463 = ORIENTED_EDGE ( 'NONE', *, *, #9804, .T. ) ;
#10464 = VERTEX_POINT ( 'NONE', #2004 ) ;
#10465 = DIRECTION ( 'NONE',  ( -0.9960067511297463483, 0.08927794634716618161, -4.818676322152979407E-17 ) ) ;
#10466 = DIRECTION ( 'NONE',  ( 1.000000000000000000, 1.665334536937735599E-15, 0.000000000000000000 ) ) ;
#10467 = CARTESIAN_POINT ( 'NONE',  ( 0.7814938847207267836, -100.6906014649701433, 7.534213779343278183 ) ) ;
#10468 = CARTESIAN_POINT ( 'NONE',  ( -0.5078243831721187540, -154.2164502162252404, -1.847253022830592561 ) ) ;
#10469 = FACE_OUTER_BOUND ( 'NONE', #4316, .T. ) ;
#10470 = EDGE_CURVE ( 'NONE', #2108, #9893, #11529, .T. ) ;
#10471 = DIRECTION ( 'NONE',  ( 1.000000000000000000, 3.568574007723717789E-15, 0.000000000000000000 ) ) ;
#10472 = FACE_OUTER_BOUND ( 'NONE', #6864, .T. ) ;
#10473 = CARTESIAN_POINT ( 'NONE',  ( 26.79177319725820539, -26.24642857144861807, -4.000000000000000000 ) ) ;
#10474 = ADVANCED_FACE ( 'NONE', ( #3117 ), #6486, .T. ) ;
#10475 = FACE_OUTER_BOUND ( 'NONE', #7815, .T. ) ;
#10476 = EDGE_CURVE ( 'NONE', #887, #9797, #13576, .T. ) ;
#10477 = DIRECTION ( 'NONE',  ( -0.8907235428302473501, 0.4545454545454531425, 0.000000000000000000 ) ) ;
#10478 = VERTEX_POINT ( 'NONE', #9845 ) ;
#10479 = DIRECTION ( 'NONE',  ( -6.158143864569485777E-17, -2.736152283717910599E-16, 1.000000000000000000 ) ) ;
#10480 = CARTESIAN_POINT ( 'NONE',  ( -35.00000000000000000, -4.286263797015736496E-15, -4.000000000000000000 ) ) ;
#10481 = CARTESIAN_POINT ( 'NONE',  ( 3.894934744998975518, -89.44155844158821367, -2.935215040338265968 ) ) ;
#10482 = ORIENTED_EDGE ( 'NONE', *, *, #9224, .F. ) ;
#10483 = CARTESIAN_POINT ( 'NONE',  ( 25.00000000000000355, 120.0000000000000142, 2.499999999999999556 ) ) ;
#10484 = ORIENTED_EDGE ( 'NONE', *, *, #11502, .F. ) ;
#10485 = DIRECTION ( 'NONE',  ( 0.000000000000000000, 0.000000000000000000, 1.000000000000000000 ) ) ;
#10486 = CARTESIAN_POINT ( 'NONE',  ( 1.187907395172932673E-14, -97.00000000000000000, 0.000000000000000000 ) ) ;
#10487 = AXIS2_PLACEMENT_3D ( 'NONE', #3008, #9532, #9257 ) ;
#10488 = CARTESIAN_POINT ( 'NONE',  ( 13.79311422413708499, -21.62638421600850691, 7.500000000000000000 ) ) ;
#10489 = CARTESIAN_POINT ( 'NONE',  ( -12.05891082652281199, -95.36363636363795138, -5.087868926931797375 ) ) ;
#10490 = AXIS2_PLACEMENT_3D ( 'NONE', #11149, #1466, #10098 ) ;
#10491 = DIRECTION ( 'NONE',  ( 0.4226182617407009401, -0.9063077870366491595, -0.000000000000000000 ) ) ;
#10492 = CARTESIAN_POINT ( 'NONE',  ( -12.99553232110414491, 48.77386654458962312, 25.99106464220826851 ) ) ;
#10493 = EDGE_CURVE ( 'NONE', #2984, #7882, #2109, .T. ) ;
#10494 = CARTESIAN_POINT ( 'NONE',  ( 15.29705854078138394, -36.87585420866476937, 30.59411708156277854 ) ) ;
#10495 = CARTESIAN_POINT ( 'NONE',  ( -4.866961404864796670, 90.10495303670558087, 1.152376359967959063 ) ) ;
#10496 = AXIS2_PLACEMENT_3D ( 'NONE', #5506, #11816, #9582 ) ;
#10497 = EDGE_LOOP ( 'NONE', ( #10774, #12220, #2940, #1949 ) ) ;
#10498 = CARTESIAN_POINT ( 'NONE',  ( -1.433044453979095634, -80.32154590898655044, 10.00519026140878864 ) ) ;
#10499 = ORIENTED_EDGE ( 'NONE', *, *, #2985, .T. ) ;
#10500 = CARTESIAN_POINT ( 'NONE',  ( 12.99579180576517423, -20.73949187309215247, 1.656338139122241719E-15 ) ) ;
#10501 = CARTESIAN_POINT ( 'NONE',  ( 31.93204061526062176, -135.0000000000000000, 3.910547132972218187E-15 ) ) ;
#10502 = CARTESIAN_POINT ( 'NONE',  ( 34.25812584745450096, 108.1980041606223466, 0.6234894336158707251 ) ) ;
#10503 = CARTESIAN_POINT ( 'NONE',  ( 35.66405164569891184, -18.73723662690267133, -2.500000000000004441 ) ) ;
#10504 = CARTESIAN_POINT ( 'NONE',  ( 1.781428662358381487, -131.6218529372965804, -3.442014977257640940 ) ) ;
#10505 = CARTESIAN_POINT ( 'NONE',  ( 35.00000000000000000, 4.286263797015736496E-15, -7.500000000000000000 ) ) ;
#10506 = ORIENTED_EDGE ( 'NONE', *, *, #12828, .T. ) ;
#10507 = CIRCLE ( 'NONE', #4030, 18.74900000001875355 ) ;
#10508 = CARTESIAN_POINT ( 'NONE',  ( 15.29705854078139460, -8.601520358636511432, 3.746698755667523200E-15 ) ) ;
#10509 = ORIENTED_EDGE ( 'NONE', *, *, #13761, .F. ) ;
#10510 = CARTESIAN_POINT ( 'NONE',  ( 0.000000000000000000, 71.01020514433645303, -7.500000000000000000 ) ) ;
#10511 = CIRCLE ( 'NONE', #1037, 25.50000000002549783 ) ;
#10512 = EDGE_LOOP ( 'NONE', ( #8375, #9260, #7294, #11020 ) ) ;
#10513 = EDGE_LOOP ( 'NONE', ( #8561, #3993, #12998, #8043 ) ) ;
#10514 = CARTESIAN_POINT ( 'NONE',  ( 12.99553232110413781, 77.04820039461787928, 1.478563310446379610E-15 ) ) ;
#10515 = EDGE_LOOP ( 'NONE', ( #7748, #4781, #7902, #2549, #9332, #12444, #9838, #5315 ) ) ;
#10516 = CARTESIAN_POINT ( 'NONE',  ( 25.00000000000001776, -100.0000000000064801, 5.046127144260958097 ) ) ;
#10517 = CARTESIAN_POINT ( 'NONE',  ( -35.00000000000000000, -4.286263797015736496E-15, 7.500000000000000000 ) ) ;
#10518 = CARTESIAN_POINT ( 'NONE',  ( 0.000000000000000000, 0.000000000000000000, 0.000000000000000000 ) ) ;
#10519 = CARTESIAN_POINT ( 'NONE',  ( -14.88155114952948921, -22.23162151614122450, -5.171026666816163520 ) ) ;
#10520 = CARTESIAN_POINT ( 'NONE',  ( 62.16766351966359849, -73.17985663200910551, 2.500000000000000000 ) ) ;
#10521 = CARTESIAN_POINT ( 'NONE',  ( 8.385254915620294014, 69.25350232273815720, -16.77050983124058448 ) ) ;
#10522 = AXIS2_PLACEMENT_3D ( 'NONE', #926, #3941, #5064 ) ;
#10523 = CARTESIAN_POINT ( 'NONE',  ( 3.721216335461446700, -108.7938388513467061, -5.424520069322383620 ) ) ;
#10524 = DIRECTION ( 'NONE',  ( -1.000000000000000000, 0.000000000000000000, 0.000000000000000000 ) ) ;
#10525 = ORIENTED_EDGE ( 'NONE', *, *, #11002, .T. ) ;
#10526 = CIRCLE ( 'NONE', #12334, 16.99999999999998934 ) ;
#10527 = ORIENTED_EDGE ( 'NONE', *, *, #13055, .F. ) ;
#10528 = AXIS2_PLACEMENT_3D ( 'NONE', #13144, #2380, #2177 ) ;
#10529 = ORIENTED_EDGE ( 'NONE', *, *, #6701, .F. ) ;
#10530 = VERTEX_POINT ( 'NONE', #7667 ) ;
#10531 = EDGE_CURVE ( 'NONE', #12589, #4671, #1681, .T. ) ;
#10532 = CARTESIAN_POINT ( 'NONE',  ( -35.00000000000000000, -4.286263797015736496E-15, 7.500000000000000000 ) ) ;
#10533 = PRODUCT_RELATED_PRODUCT_CATEGORY ( 'part', '', ( #3279 ) ) ;
#10534 = CARTESIAN_POINT ( 'NONE',  ( 50.89489709276795537, 9.943703908052052398, -2.499999999999994671 ) ) ;
#10535 = CARTESIAN_POINT ( 'NONE',  ( 2.780317640840915594, -98.85838219806488780, 7.289431051163909991 ) ) ;
#10536 = VECTOR ( 'NONE', #9167, 1000.000000000000000 ) ;
#10537 = TOROIDAL_SURFACE ( 'NONE', #12799, 16.99999999999998934, 2.000000000000000000 ) ;
#10538 = CYLINDRICAL_SURFACE ( 'NONE', #1106, 9.000000000008999024 ) ;
#10539 = CARTESIAN_POINT ( 'NONE',  ( 15.29705854078139460, 64.91013567203349055, -30.59411708156277854 ) ) ;
#10540 = DIRECTION ( 'NONE',  ( -1.000000000000000000, 0.000000000000000000, 0.000000000000000000 ) ) ;
#10541 = CARTESIAN_POINT ( 'NONE',  ( 28.15981099771517648, -27.70535714287384721, 4.000000000000000000 ) ) ;
#10542 = DIRECTION ( 'NONE',  ( 0.000000000000000000, 0.000000000000000000, 1.000000000000000000 ) ) ;
#10543 = CARTESIAN_POINT ( 'NONE',  ( 8.385254915620292238, 69.25350232273815720, 9.022884433393300556E-16 ) ) ;
#10544 = VECTOR ( 'NONE', #8847, 1000.000000000000000 ) ;
#10545 = CARTESIAN_POINT ( 'NONE',  ( 31.01425004688410070, -18.32044754671509423, -2.500000000000004441 ) ) ;
#10546 = AXIS2_PLACEMENT_3D ( 'NONE', #11491, #1881, #6169 ) ;
#10547 = EDGE_CURVE ( 'NONE', #3686, #13516, #4099, .T. ) ;
#10548 = LINE ( 'NONE', #1018, #13281 ) ;
#10549 = DIRECTION ( 'NONE',  ( -6.158143864569485777E-17, -2.736152283717910599E-16, 1.000000000000000000 ) ) ;
#10550 = CARTESIAN_POINT ( 'NONE',  ( 6.062451257354256384, -129.7272727272775512, -11.56901651898783001 ) ) ;
#10551 = EDGE_CURVE ( 'NONE', #42, #131, #7044, .T. ) ;
#10552 = ORIENTED_EDGE ( 'NONE', *, *, #7222, .F. ) ;
#10553 = CARTESIAN_POINT ( 'NONE',  ( 15.29705854078138749, -10.48808792804187284, 30.59411708156277854 ) ) ;
#10554 = EDGE_CURVE ( 'NONE', #11257, #5704, #7595, .T. ) ;
#10555 = ORIENTED_EDGE ( 'NONE', *, *, #4190, .F. ) ;
#10556 = CYLINDRICAL_SURFACE ( 'NONE', #12892, 24.99999999999998934 ) ;
#10557 = EDGE_CURVE ( 'NONE', #1069, #9187, #4568, .T. ) ;
#10558 = DIRECTION ( 'NONE',  ( -1.224646799147353207E-16, 1.000000000000000000, -0.000000000000000000 ) ) ;
#10559 = CARTESIAN_POINT ( 'NONE',  ( 7.328281203649089193, -76.12121211817229494, 4.753922619608384359 ) ) ;
#10560 = CARTESIAN_POINT ( 'NONE',  ( -2.247751904815863622, -65.63636362841093330, 0.1634371276632270997 ) ) ;
#10561 = AXIS2_PLACEMENT_3D ( 'NONE', #1336, #9760, #2539 ) ;
#10562 = CARTESIAN_POINT ( 'NONE',  ( 15.18222645069203303, -16.04698886238941924, 4.000000000000000000 ) ) ;
#10563 = CARTESIAN_POINT ( 'NONE',  ( 10.69381717166375800, -21.56444287793185666, 2.619229793989004345E-15 ) ) ;
#10564 = CARTESIAN_POINT ( 'NONE',  ( -15.29705854078139282, -36.87585420866476937, 30.59411708156277498 ) ) ;
#10565 = CARTESIAN_POINT ( 'NONE',  ( -4.367873154833913141, 91.47215508561177444, 2.433639722925613924 ) ) ;
#10566 = ORIENTED_EDGE ( 'NONE', *, *, #8259, .T. ) ;
#10567 = EDGE_CURVE ( 'NONE', #13160, #6892, #339, .T. ) ;
#10568 = CIRCLE ( 'NONE', #511, 8.385254915620290461 ) ;
#10569 = EDGE_CURVE ( 'NONE', #6314, #7422, #5465, .T. ) ;
#10570 = ORIENTED_EDGE ( 'NONE', *, *, #701, .F. ) ;
#10571 = CARTESIAN_POINT ( 'NONE',  ( 8.385254915620295790, -12.94488700934118341, -16.77050983124058448 ) ) ;
#10572 = CARTESIAN_POINT ( 'NONE',  ( -8.385254915620295790, 69.25350232273815720, -1.271481101603046320E-15 ) ) ;
#10573 = CARTESIAN_POINT ( 'NONE',  ( -15.29705854078139815, 55.48535772202409788, 30.59411708156277854 ) ) ;
#10574 = LINE ( 'NONE', #10308, #1798 ) ;
#10575 = CARTESIAN_POINT ( 'NONE',  ( 0.4884533741263017981, -128.8023475767107016, -4.172574844680278616 ) ) ;
#10576 = LINE ( 'NONE', #713, #7789 ) ;
#10577 = ORIENTED_EDGE ( 'NONE', *, *, #11330, .F. ) ;
#10578 = ORIENTED_EDGE ( 'NONE', *, *, #7132, .F. ) ;
#10579 = ORIENTED_EDGE ( 'NONE', *, *, #9562, .F. ) ;
#10580 =( BOUNDED_SURFACE ( )  B_SPLINE_SURFACE ( 3, 3, ( 
 ( #498, #4760, #4963, #9242 ),
 ( #13348, #3908, #7982, #12260 ),
 ( #11341, #2647, #564, #4830 ),
 ( #13421, #12332, #1799, #8187 ) ),
 .UNSPECIFIED., .F., .F., .F. ) 
 B_SPLINE_SURFACE_WITH_KNOTS ( ( 4, 4 ),
 ( 4, 4 ),
 ( 0.000000000000000000, 1.000000000000000000 ),
 ( 0.000000000000000000, 1.000000000000000000 ),
 .UNSPECIFIED. ) 
 GEOMETRIC_REPRESENTATION_ITEM ( )  RATIONAL_B_SPLINE_SURFACE ( (
 ( 1.000000000000000000, 0.3333333333333334259, 0.3333333333333334259, 1.000000000000000000),
 ( 1.000000000000000000, 0.3333333333333334259, 0.3333333333333334259, 1.000000000000000000),
 ( 1.000000000000000000, 0.3333333333333334259, 0.3333333333333334259, 1.000000000000000000),
 ( 1.000000000000000000, 0.3333333333333334259, 0.3333333333333334259, 1.000000000000000000) ) ) 
 REPRESENTATION_ITEM ( '' )  SURFACE ( )  );
#10581 = AXIS2_PLACEMENT_3D ( 'NONE', #2219, #4527, #5515 ) ;
#10582 = EDGE_CURVE ( 'NONE', #618, #8349, #8945, .T. ) ;
#10583 = DIRECTION ( 'NONE',  ( -0.000000000000000000, -0.000000000000000000, -1.000000000000000000 ) ) ;
#10584 = ORIENTED_EDGE ( 'NONE', *, *, #5847, .F. ) ;
#10585 = CARTESIAN_POINT ( 'NONE',  ( -15.29705854078138394, -38.76242177807012723, -30.59411708156277854 ) ) ;
#10586 = ORIENTED_EDGE ( 'NONE', *, *, #12304, .F. ) ;
#10587 = DIRECTION ( 'NONE',  ( 0.000000000000000000, 0.000000000000000000, 1.000000000000000000 ) ) ;
#10588 = CARTESIAN_POINT ( 'NONE',  ( 36.36363636363638108, 142.2680885707561629, 0.5000000000000000000 ) ) ;
#10589 = CARTESIAN_POINT ( 'NONE',  ( -15.70089697932619899, -22.78139155752743861, 0.6412871628180817352 ) ) ;
#10590 = CARTESIAN_POINT ( 'NONE',  ( -24.99999999999998224, -99.22499053259343782, 1.700537903188983346 ) ) ;
#10591 = DIRECTION ( 'NONE',  ( -0.4545454545454548634, 0.8907235428302464619, 0.000000000000000000 ) ) ;
#10592 = VECTOR ( 'NONE', #11613, 1000.000000000000000 ) ;
#10593 = CARTESIAN_POINT ( 'NONE',  ( -1.952880862260572670, -132.1386478743458781, 3.257033108385012365 ) ) ;
#10594 = DIRECTION ( 'NONE',  ( 0.000000000000000000, 1.000000000000000000, -0.000000000000000000 ) ) ;
#10595 = ORIENTED_EDGE ( 'NONE', *, *, #13794, .F. ) ;
#10596 = ORIENTED_EDGE ( 'NONE', *, *, #255, .F. ) ;
#10597 = ORIENTED_EDGE ( 'NONE', *, *, #7805, .F. ) ;
#10598 = CARTESIAN_POINT ( 'NONE',  ( -1.246623049074521372, -140.6414058277869970, -2.594349448477115683 ) ) ;
#10599 = VECTOR ( 'NONE', #923, 1000.000000000000000 ) ;
#10600 = CIRCLE ( 'NONE', #13562, 9.000000000008999024 ) ;
#10601 = DIRECTION ( 'NONE',  ( 0.000000000000000000, 0.000000000000000000, 1.000000000000000000 ) ) ;
#10602 = DIRECTION ( 'NONE',  ( -1.000000000000000000, 0.000000000000000000, 0.000000000000000000 ) ) ;
#10603 = CARTESIAN_POINT ( 'NONE',  ( -5.190364408751921843, -107.5279543462731056, 4.303367517544086418 ) ) ;
#10604 = DIRECTION ( 'NONE',  ( 0.9960067511297463483, -0.08927794634716620936, 4.818676322152979407E-17 ) ) ;
#10605 = CARTESIAN_POINT ( 'NONE',  ( 76.84607712649204814, -99.92541302764922762, -2.500000000000000000 ) ) ;
#10606 = CARTESIAN_POINT ( 'NONE',  ( -8.385254915620294014, 22.12961257269105531, -2.113820870476202140E-15 ) ) ;
#10607 = EDGE_CURVE ( 'NONE', #9642, #2556, #5766, .T. ) ;
#10608 = CARTESIAN_POINT ( 'NONE',  ( 25.00000000000001776, -100.0000000000000000, -5.046127144242417373 ) ) ;
#10609 = FACE_OUTER_BOUND ( 'NONE', #13793, .T. ) ;
#10610 = VECTOR ( 'NONE', #2675, 1000.000000000000000 ) ;
#10611 = LINE ( 'NONE', #1996, #237 ) ;
#10612 = CARTESIAN_POINT ( 'NONE',  ( -4.980291965142432886, -118.2727272727225483, -1.265069668247100543 ) ) ;
#10613 = ORIENTED_EDGE ( 'NONE', *, *, #11278, .T. ) ;
#10614 = DIRECTION ( 'NONE',  ( 1.000000000000000000, 1.850371707708595154E-15, 0.000000000000000000 ) ) ;
#10615 = EDGE_LOOP ( 'NONE', ( #11365, #5071, #5917, #11248 ) ) ;
#10616 = CIRCLE ( 'NONE', #9729, 25.50418395392908977 ) ;
#10617 = DIRECTION ( 'NONE',  ( 1.000000000000000000, 0.000000000000000000, 0.000000000000000000 ) ) ;
#10618 = CARTESIAN_POINT ( 'NONE',  ( -30.72062512117240018, 25.13835616439069653, 4.000000000000000000 ) ) ;
#10619 = CARTESIAN_POINT ( 'NONE',  ( 13.79311422413708499, -21.62638421600850691, -7.500000000000000000 ) ) ;
#10620 = CARTESIAN_POINT ( 'NONE',  ( 8.931512003261595112, -153.6493506494127814, -10.28374512068234559 ) ) ;
#10621 = EDGE_CURVE ( 'NONE', #10825, #6779, #3016, .T. ) ;
#10622 = CARTESIAN_POINT ( 'NONE',  ( -15.29705854078139105, -10.48808792804187284, 1.852046186812095429E-17 ) ) ;
#10623 = CARTESIAN_POINT ( 'NONE',  ( 12.99553232110414314, 11.07475474455194053, -25.99106464220826851 ) ) ;
#10624 = EDGE_CURVE ( 'NONE', #5941, #11307, #12664, .T. ) ;
#10625 = CARTESIAN_POINT ( 'NONE',  ( -35.00000000000000000, -4.286263797015736496E-15, -10.49999999999999822 ) ) ;
#10626 = CYLINDRICAL_SURFACE ( 'NONE', #13768, 5.000000000000000000 ) ;
#10627 = DIRECTION ( 'NONE',  ( 0.000000000000000000, 0.000000000000000000, 1.000000000000000000 ) ) ;
#10628 = EDGE_CURVE ( 'NONE', #6696, #7751, #5698, .T. ) ;
#10629 = AXIS2_PLACEMENT_3D ( 'NONE', #11322, #11383, #12244 ) ;
#10630 = EDGE_CURVE ( 'NONE', #4461, #12007, #13023, .T. ) ;
#10631 = ORIENTED_EDGE ( 'NONE', *, *, #3630, .T. ) ;
#10632 = DIRECTION ( 'NONE',  ( 0.000000000000000000, 0.000000000000000000, 1.000000000000000000 ) ) ;
#10633 = ORIENTED_EDGE ( 'NONE', *, *, #5943, .F. ) ;
#10634 = FACE_OUTER_BOUND ( 'NONE', #8258, .T. ) ;
#10635 = AXIS2_PLACEMENT_3D ( 'NONE', #10058, #5927, #13241 ) ;
#10636 = DIRECTION ( 'NONE',  ( -0.000000000000000000, -0.000000000000000000, -1.000000000000000000 ) ) ;
#10637 = CARTESIAN_POINT ( 'NONE',  ( -15.29705854078138394, 29.09759144140119957, -30.59411708156277854 ) ) ;
#10638 =( GEOMETRIC_REPRESENTATION_CONTEXT ( 3 ) GLOBAL_UNCERTAINTY_ASSIGNED_CONTEXT ( ( #7832 ) ) GLOBAL_UNIT_ASSIGNED_CONTEXT ( ( #6812, #1332, #6595 ) ) REPRESENTATION_CONTEXT ( 'NONE', 'WORKASPACE' ) );
#10639 = AXIS2_PLACEMENT_3D ( 'NONE', #13859, #7638, #1068 ) ;
#10640 = DIRECTION ( 'NONE',  ( -2.797435172181481150E-17, 1.000000000000000000, -1.765856845898762549E-18 ) ) ;
#10641 =( NAMED_UNIT ( * ) SI_UNIT ( $, .STERADIAN. ) SOLID_ANGLE_UNIT ( ) );
#10642 = DIRECTION ( 'NONE',  ( 0.000000000000000000, 0.000000000000000000, 1.000000000000000000 ) ) ;
#10643 = EDGE_CURVE ( 'NONE', #10377, #7475, #1356, .T. ) ;
#10644 = ORIENTED_EDGE ( 'NONE', *, *, #5335, .F. ) ;
#10645 = EDGE_CURVE ( 'NONE', #4466, #12157, #5705, .T. ) ;
#10646 = CIRCLE ( 'NONE', #5718, 5.000000000000004441 ) ;
#10647 = VECTOR ( 'NONE', #4548, 1000.000000000000000 ) ;
#10648 = DIRECTION ( 'NONE',  ( -2.797435172181481150E-17, 1.000000000000000000, -1.765856845898762549E-18 ) ) ;
#10649 = CARTESIAN_POINT ( 'NONE',  ( 9.701113296676155073, -69.00000000000008527, 3.021359762293434503 ) ) ;
#10650 = ORIENTED_EDGE ( 'NONE', *, *, #3780, .F. ) ;
#10651 = CARTESIAN_POINT ( 'NONE',  ( -10.69381717166375623, 72.68333662216238622, -1.566311632108520979E-15 ) ) ;
#10652 = DIRECTION ( 'NONE',  ( -0.4545454545454531425, -0.8907235428302472391, 0.000000000000000000 ) ) ;
#10653 = CIRCLE ( 'NONE', #5504, 18.74900000001875000 ) ;
#10654 = DIRECTION ( 'NONE',  ( -1.000000000000000000, 0.000000000000000000, 0.000000000000000000 ) ) ;
#10655 = CARTESIAN_POINT ( 'NONE',  ( 40.33442208022854913, 100.7954446087837823, -1.738653613625530614 ) ) ;
#10656 = CARTESIAN_POINT ( 'NONE',  ( 12.99553232110413781, 67.62342244460847951, 1.492702117415814531E-15 ) ) ;
#10657 = CARTESIAN_POINT ( 'NONE',  ( 0.07095332755016135751, -158.6814110685799051, -1.494078031317318755 ) ) ;
#10658 = DIRECTION ( 'NONE',  ( -6.158143864569485777E-17, -2.736152283717910599E-16, 1.000000000000000000 ) ) ;
#10659 = ORIENTED_EDGE ( 'NONE', *, *, #9461, .T. ) ;
#10660 = EDGE_CURVE ( 'NONE', #12400, #11019, #3385, .T. ) ;
#10661 = VERTEX_POINT ( 'NONE', #6837 ) ;
#10662 = EDGE_LOOP ( 'NONE', ( #8831, #5965 ) ) ;
#10663 = VECTOR ( 'NONE', #5164, 1000.000000000000000 ) ;
#10664 = PRODUCT_DEFINITION_SHAPE ( 'NONE', 'NONE',  #3939 ) ;
#10665 = CARTESIAN_POINT ( 'NONE',  ( 50.00000000000000000, 120.0000000000000142, -0.5000000000000000000 ) ) ;
#10666 = ORIENTED_EDGE ( 'NONE', *, *, #3093, .F. ) ;
#10667 = CARTESIAN_POINT ( 'NONE',  ( -12.99553232110413781, 39.34908859458022334, -3.265581959298969830E-15 ) ) ;
#10668 = CARTESIAN_POINT ( 'NONE',  ( -2.094721958917744153, -120.2871812560114506, -4.762225812260485469 ) ) ;
#10669 = CARTESIAN_POINT ( 'NONE',  ( 15.29705854078139815, -8.601520358636511432, -30.59411708156277854 ) ) ;
#10670 = CARTESIAN_POINT ( 'NONE',  ( 1.109824446840197210, -148.3982683987656799, -1.619194360870498173 ) ) ;
#10671 = CARTESIAN_POINT ( 'NONE',  ( -12.99579180576516535, 64.08350967699263379, -25.99158361153034136 ) ) ;
#10672 = CARTESIAN_POINT ( 'NONE',  ( -30.68181818181819054, 131.1340442853780814, 7.500000000000000000 ) ) ;
#10673 = CARTESIAN_POINT ( 'NONE',  ( -7.783279735887626671, -74.45454545454313688, -6.359494517302866967 ) ) ;
#10674 = CARTESIAN_POINT ( 'NONE',  ( 25.00000000000001776, -100.0000000000000000, 7.500000000000000000 ) ) ;
#10675 = DIRECTION ( 'NONE',  ( -0.000000000000000000, -0.000000000000000000, -1.000000000000000000 ) ) ;
#10676 = CARTESIAN_POINT ( 'NONE',  ( -25.00000000000000355, 120.0000000000000142, -2.500000000000000000 ) ) ;
#10677 = CARTESIAN_POINT ( 'NONE',  ( -25.00000000000000355, 120.0000000000000142, 0.5000000000000000000 ) ) ;
#10678 = ORIENTED_EDGE ( 'NONE', *, *, #2327, .T. ) ;
#10679 = VERTEX_POINT ( 'NONE', #11032 ) ;
#10680 = CARTESIAN_POINT ( 'NONE',  ( 8.385254915620294014, 24.75422479069652582, 9.855024866598292994E-16 ) ) ;
#10681 = VERTEX_POINT ( 'NONE', #11116 ) ;
#10682 = DIRECTION ( 'NONE',  ( 1.000000000000000000, 0.000000000000000000, 0.000000000000000000 ) ) ;
#10683 = CARTESIAN_POINT ( 'NONE',  ( -35.00000000000000000, -4.286263797015736496E-15, 7.500000000000000000 ) ) ;
#10684 = CARTESIAN_POINT ( 'NONE',  ( 12.99579180576516180, 26.38439787695498495, 25.99158361153033425 ) ) ;
#10685 = DIRECTION ( 'NONE',  ( 1.000000000000000000, -0.000000000000000000, -0.000000000000000000 ) ) ;
#10686 = CARTESIAN_POINT ( 'NONE',  ( -36.36363636363635976, 142.2680885707561629, 0.5000000000000000000 ) ) ;
#10687 = CARTESIAN_POINT ( 'NONE',  ( -12.99579180576517068, 26.38439787695498495, -3.233995902620226781E-15 ) ) ;
#10688 = DIRECTION ( 'NONE',  ( 0.9960067511297464593, -0.08927794634716622324, 3.401418580343279473E-17 ) ) ;
#10689 = CARTESIAN_POINT ( 'NONE',  ( 31.81818181818183433, 133.3608531424536920, 2.500000000000000000 ) ) ;
#10690 = VECTOR ( 'NONE', #6304, 1000.000000000000000 ) ;
#10691 = PLANE ( 'NONE',  #11836 ) ;
#10692 = VERTEX_POINT ( 'NONE', #1502 ) ;
#10693 = EDGE_CURVE ( 'NONE', #4720, #2860, #12215, .T. ) ;
#10694 = ADVANCED_FACE ( 'NONE', ( #3956 ), #5783, .F. ) ;
#10695 = VERTEX_POINT ( 'NONE', #2837 ) ;
#10696 = FACE_OUTER_BOUND ( 'NONE', #4248, .T. ) ;
#10697 = DIRECTION ( 'NONE',  ( 0.000000000000000000, 0.000000000000000000, 1.000000000000000000 ) ) ;
#10698 = CARTESIAN_POINT ( 'NONE',  ( 53.02537423504344360, -5.158573900538657497, -2.499999999999999112 ) ) ;
#10699 = CARTESIAN_POINT ( 'NONE',  ( -10.07809618140513663, -70.83793457579116648, -0.9291402644571875591 ) ) ;
#10700 = FACE_OUTER_BOUND ( 'NONE', #3804, .T. ) ;
#10701 = AXIS2_PLACEMENT_3D ( 'NONE', #8207, #5048, #1821 ) ;
#10702 = DIRECTION ( 'NONE',  ( -2.797435172181481150E-17, 1.000000000000000000, -1.765856845898762549E-18 ) ) ;
#10703 = ORIENTED_EDGE ( 'NONE', *, *, #13052, .T. ) ;
#10704 = ORIENTED_EDGE ( 'NONE', *, *, #5677, .T. ) ;
#10705 = EDGE_CURVE ( 'NONE', #6547, #5305, #1574, .T. ) ;
#10706 = ADVANCED_FACE ( 'NONE', ( #610 ), #12448, .T. ) ;
#10707 = EDGE_CURVE ( 'NONE', #12700, #6483, #13686, .T. ) ;
#10708 = ORIENTED_EDGE ( 'NONE', *, *, #5903, .F. ) ;
#10709 = ORIENTED_EDGE ( 'NONE', *, *, #7631, .T. ) ;
#10710 = EDGE_CURVE ( 'NONE', #12810, #13223, #10418, .T. ) ;
#10711 = LINE ( 'NONE', #12048, #13274 ) ;
#10712 = EDGE_CURVE ( 'NONE', #3748, #5379, #2318, .T. ) ;
#10713 = DIRECTION ( 'NONE',  ( 0.7999999999999999334, -0.6000000000000001998, 0.000000000000000000 ) ) ;
#10714 = CARTESIAN_POINT ( 'NONE',  ( -3.656918945275430932, -76.68408302446904656, -9.436988915889060081 ) ) ;
#10715 = DIRECTION ( 'NONE',  ( -2.797435172181481150E-17, 1.000000000000000000, -1.765856845898762549E-18 ) ) ;
#10716 = DIRECTION ( 'NONE',  ( 0.8907235428302465730, 0.4545454545454549189, 0.000000000000000000 ) ) ;
#10717 = CARTESIAN_POINT ( 'NONE',  ( -6.423503816350314644, -86.98444705607441563, 6.714555888684349050 ) ) ;
#10718 = DIRECTION ( 'NONE',  ( 0.000000000000000000, 0.000000000000000000, 1.000000000000000000 ) ) ;
#10719 = ORIENTED_EDGE ( 'NONE', *, *, #3334, .T. ) ;
#10720 = AXIS2_PLACEMENT_3D ( 'NONE', #4410, #8694, #3645 ) ;
#10721 = EDGE_LOOP ( 'NONE', ( #463, #11518, #13165, #5631 ) ) ;
#10722 = ORIENTED_EDGE ( 'NONE', *, *, #6851, .T. ) ;
#10723 = AXIS2_PLACEMENT_3D ( 'NONE', #2783, #10148, #9094 ) ;
#10724 = ADVANCED_FACE ( 'NONE', ( #11791 ), #11402, .T. ) ;
#10725 = CARTESIAN_POINT ( 'NONE',  ( -3.286535165834789662, 90.13351245737436557, 3.771524672989932547 ) ) ;
#10726 = CARTESIAN_POINT ( 'NONE',  ( 34.99999999999958789, 1.104930248025249758E-13, -2.499999999999999112 ) ) ;
#10727 = ORIENTED_EDGE ( 'NONE', *, *, #11315, .F. ) ;
#10728 = CARTESIAN_POINT ( 'NONE',  ( 15.29705854078139282, -1.063309978032445091, 3.746698755667523200E-15 ) ) ;
#10729 = CARTESIAN_POINT ( 'NONE',  ( 15.29705854078138572, 38.52236939141059935, 1.806990092252540040E-15 ) ) ;
#10730 = DIRECTION ( 'NONE',  ( 0.7627754036039197105, 0.6466635011015212653, 0.000000000000000000 ) ) ;
#10731 = ADVANCED_FACE ( 'NONE', ( #9903 ), #13079, .T. ) ;
#10732 = CARTESIAN_POINT ( 'NONE',  ( 16.85679715600144135, -10.85606698379831947, -2.500000000000003553 ) ) ;
#10733 = AXIS2_PLACEMENT_3D ( 'NONE', #13406, #4740, #10206 ) ;
#10734 = CARTESIAN_POINT ( 'NONE',  ( 25.00000000000000355, 120.0000000000000142, 2.500000000000000000 ) ) ;
#10735 = CARTESIAN_POINT ( 'NONE',  ( 41.99999999999999289, 120.0000000000000142, -2.500000000000000000 ) ) ;
#10736 = CARTESIAN_POINT ( 'NONE',  ( 32.95454545454546036, 135.5876619995293026, 2.499999999999999556 ) ) ;
#10737 = CIRCLE ( 'NONE', #4032, 72.49999999999998579 ) ;
#10738 = CARTESIAN_POINT ( 'NONE',  ( 2.224254061606619093, -80.66666666666661456, -9.925145656127773108 ) ) ;
#10739 = CIRCLE ( 'NONE', #4465, 8.385254915620292238 ) ;
#10740 = CARTESIAN_POINT ( 'NONE',  ( -10.69346802281034670, -16.37459952631584059, -1.251741741247135829E-15 ) ) ;
#10741 = DIRECTION ( 'NONE',  ( -6.158143864569485777E-17, -2.736152283717910599E-16, 1.000000000000000000 ) ) ;
#10742 = ORIENTED_EDGE ( 'NONE', *, *, #1818, .F. ) ;
#10743 = CARTESIAN_POINT ( 'NONE',  ( 0.000000000000000000, -20.00000000000000355, 0.000000000000000000 ) ) ;
#10744 = LINE ( 'NONE', #1221, #2012 ) ;
#10745 = CIRCLE ( 'NONE', #692, 8.385254915620294014 ) ;
#10746 = ORIENTED_EDGE ( 'NONE', *, *, #3677, .F. ) ;
#10747 = AXIS2_PLACEMENT_3D ( 'NONE', #12516, #13397, #13317 ) ;
#10748 = CARTESIAN_POINT ( 'NONE',  ( 47.49999999999999289, 120.0000000000000142, 7.500000000000000000 ) ) ;
#10749 = EDGE_LOOP ( 'NONE', ( #10482, #3660, #6447, #2896, #441, #7732 ) ) ;
#10750 = CYLINDRICAL_SURFACE ( 'NONE', #13809, 25.50000000002549783 ) ;
#10751 = DIRECTION ( 'NONE',  ( -1.000000000000000000, 0.000000000000000000, 0.000000000000000000 ) ) ;
#10752 = DIRECTION ( 'NONE',  ( -6.158143864569485777E-17, -2.736152283717910599E-16, 1.000000000000000000 ) ) ;
#10753 = CARTESIAN_POINT ( 'NONE',  ( 34.78790783510986984, 106.9804631782721884, -2.384639261440465674 ) ) ;
#10754 = CIRCLE ( 'NONE', #2719, 11.81226048336476886 ) ;
#10755 = CARTESIAN_POINT ( 'NONE',  ( -12.99579180576516535, 26.38439787695498495, -25.99158361153034136 ) ) ;
#10756 = FACE_OUTER_BOUND ( 'NONE', #7067, .T. ) ;
#10757 =( GEOMETRIC_REPRESENTATION_CONTEXT ( 3 ) GLOBAL_UNCERTAINTY_ASSIGNED_CONTEXT ( ( #6570 ) ) GLOBAL_UNIT_ASSIGNED_CONTEXT ( ( #12413, #10022, #6101 ) ) REPRESENTATION_CONTEXT ( 'NONE', 'WORKASPACE' ) );
#10758 = DIRECTION ( 'NONE',  ( -1.000000000000000000, 0.000000000000000000, 0.000000000000000000 ) ) ;
#10759 = B_SPLINE_CURVE_WITH_KNOTS ( 'NONE', 3,
 ( #11120, #7891, #2087, #12839, #1437, #8951, #5311, #5243, #3205, #9591, #5714, #13257, #10770, #6197, #9528, #7483, #2152, #6437, #8872, #13182, #10699, #12172, #13840, #12098 ),
 .UNSPECIFIED., .F., .F.,
 ( 4, 2, 2, 2, 2, 2, 2, 2, 2, 2, 2, 4 ),
 ( 0.000000000000000000, 0.002159622253435538111, 0.003239433380153306733, 0.004319244506871076222, 0.006478866760306590915, 0.008638489013742107342, 0.01079811126717762637, 0.01295773352061314540, 0.01403754464733089277, 0.01511735577404864188, 0.01619716690076638752, 0.01727697802748413489 ),
 .UNSPECIFIED. ) ;
#10760 = VECTOR ( 'NONE', #11316, 1000.000000000000000 ) ;
#10761 = CARTESIAN_POINT ( 'NONE',  ( -1.747091603990086329E-15, 62.45333659073423860, -1.102836519679677113E-16 ) ) ;
#10762 = B_SPLINE_CURVE_WITH_KNOTS ( 'NONE', 3,
 ( #4902, #11354, #7923, #12349 ),
 .UNSPECIFIED., .F., .F.,
 ( 4, 4 ),
 ( 0.000000000000000000, 1.000000000000000000 ),
 .UNSPECIFIED. ) ;
#10763 = VERTEX_POINT ( 'NONE', #169 ) ;
#10764 = APPLICATION_CONTEXT ( 'automotive_design' ) ;
#10765 = ORIENTED_EDGE ( 'NONE', *, *, #9361, .F. ) ;
#10766 = CIRCLE ( 'NONE', #10561, 18.74900000001875711 ) ;
#10767 = ORIENTED_EDGE ( 'NONE', *, *, #12699, .T. ) ;
#10768 = DIRECTION ( 'NONE',  ( -0.2228746399763467390, 0.9748471135800802490, 2.409338161076489210E-16 ) ) ;
#10769 = DIRECTION ( 'NONE',  ( 0.000000000000000000, 0.000000000000000000, 1.000000000000000000 ) ) ;
#10770 = CARTESIAN_POINT ( 'NONE',  ( -8.557187102284723679, -74.11437728923387169, -5.386762695872780782 ) ) ;
#10771 = CARTESIAN_POINT ( 'NONE',  ( -25.00000000000000355, 120.0000000000000142, 2.500000000000000000 ) ) ;
#10772 = EDGE_CURVE ( 'NONE', #11806, #4480, #9082, .T. ) ;
#10773 = CARTESIAN_POINT ( 'NONE',  ( -35.00000000000000000, -20.00000000000000000, -7.500000000000000000 ) ) ;
#10774 = ORIENTED_EDGE ( 'NONE', *, *, #1141, .T. ) ;
#10775 = ORIENTED_EDGE ( 'NONE', *, *, #8816, .F. ) ;
#10776 = ORIENTED_EDGE ( 'NONE', *, *, #13514, .T. ) ;
#10777 = DIRECTION ( 'NONE',  ( 0.000000000000000000, 0.000000000000000000, 1.000000000000000000 ) ) ;
#10778 = DIRECTION ( 'NONE',  ( 1.000000000000000000, 0.000000000000000000, 0.000000000000000000 ) ) ;
#10779 = CARTESIAN_POINT ( 'NONE',  ( -6.850226882306651000, -73.90543885042040984, -7.468286930689518321 ) ) ;
#10780 = CARTESIAN_POINT ( 'NONE',  ( -34.92076574184287097, 106.7798134293913961, -2.447438947438305590 ) ) ;
#10781 = CARTESIAN_POINT ( 'NONE',  ( -15.29705854078138394, 66.79670324143890525, -30.59411708156277498 ) ) ;
#10782 = ADVANCED_FACE ( 'NONE', ( #10795 ), #3032, .T. ) ;
#10783 = CARTESIAN_POINT ( 'NONE',  ( 1.574536146393409775, -80.31525646925749129, 9.985167164889261926 ) ) ;
#10784 = EDGE_CURVE ( 'NONE', #8899, #768, #9758, .T. ) ;
#10785 = DIRECTION ( 'NONE',  ( 0.000000000000000000, 0.000000000000000000, 1.000000000000000000 ) ) ;
#10786 = EDGE_CURVE ( 'NONE', #4611, #13845, #2116, .T. ) ;
#10787 = ORIENTED_EDGE ( 'NONE', *, *, #2870, .F. ) ;
#10788 = VERTEX_POINT ( 'NONE', #12935 ) ;
#10789 = ORIENTED_EDGE ( 'NONE', *, *, #11862, .F. ) ;
#10790 = ADVANCED_FACE ( 'NONE', ( #5406 ), #8530, .T. ) ;
#10791 = ADVANCED_FACE ( 'NONE', ( #5761 ), #447, .T. ) ;
#10792 = CARTESIAN_POINT ( 'NONE',  ( -25.00000000000000355, 120.0000000000000142, -2.499999999999998668 ) ) ;
#10793 = ORIENTED_EDGE ( 'NONE', *, *, #9722, .T. ) ;
#10794 = CARTESIAN_POINT ( 'NONE',  ( 15.29705854078139815, 90.00000000000000000, 1.714422261702873752E-15 ) ) ;
#10795 = FACE_OUTER_BOUND ( 'NONE', #8737, .T. ) ;
#10796 = CARTESIAN_POINT ( 'NONE',  ( 1.387778780781445676E-14, -135.0000000000000000, 0.000000000000000000 ) ) ;
#10797 = AXIS2_PLACEMENT_3D ( 'NONE', #1602, #3841, #5887 ) ;
#10798 = DIRECTION ( 'NONE',  ( 0.000000000000000000, 0.000000000000000000, 1.000000000000000000 ) ) ;
#10799 = CARTESIAN_POINT ( 'NONE',  ( -1.956031471770462549, -154.2164502162973747, -1.283490743970612025 ) ) ;
#10800 = CARTESIAN_POINT ( 'NONE',  ( -8.627629343136057116, -71.90909090909200074, -5.462837922541642577 ) ) ;
#10801 = CARTESIAN_POINT ( 'NONE',  ( 34.99999999999958789, 1.104930248025249758E-13, -2.499999999999999112 ) ) ;
#10802 = DIRECTION ( 'NONE',  ( -0.000000000000000000, -0.000000000000000000, -1.000000000000000000 ) ) ;
#10803 = VECTOR ( 'NONE', #13377, 1000.000000000000000 ) ;
#10804 = EDGE_LOOP ( 'NONE', ( #9622, #5993, #10950, #6593 ) ) ;
#10805 = EDGE_CURVE ( 'NONE', #7777, #7988, #1909, .T. ) ;
#10806 = CARTESIAN_POINT ( 'NONE',  ( 4.330127018922190985, 92.00000000000000000, 2.500000000000000000 ) ) ;
#10807 = DIRECTION ( 'NONE',  ( -0.000000000000000000, -0.000000000000000000, -1.000000000000000000 ) ) ;
#10808 = EDGE_LOOP ( 'NONE', ( #2658, #3157, #6589, #9249 ) ) ;
#10809 = CARTESIAN_POINT ( 'NONE',  ( 22.00707094244967621, -21.94159963418280412, -2.500000000000005329 ) ) ;
#10810 = DIRECTION ( 'NONE',  ( 0.000000000000000000, -0.000000000000000000, 1.000000000000000000 ) ) ;
#10811 = ORIENTED_EDGE ( 'NONE', *, *, #2592, .T. ) ;
#10812 = CARTESIAN_POINT ( 'NONE',  ( 15.29705854078139460, -18.02629830864596627, 1.906846944237139921E-15 ) ) ;
#10813 = ORIENTED_EDGE ( 'NONE', *, *, #10885, .F. ) ;
#10814 = DIRECTION ( 'NONE',  ( -0.000000000000000000, -0.000000000000000000, -1.000000000000000000 ) ) ;
#10815 = CARTESIAN_POINT ( 'NONE',  ( -12.99579180576517068, 54.65873172698324112, -3.291435486758484277E-15 ) ) ;
#10816 = AXIS2_PLACEMENT_3D ( 'NONE', #6814, #11011, #5836 ) ;
#10817 = AXIS2_PLACEMENT_3D ( 'NONE', #4744, #11193, #2977 ) ;
#10818 = DIRECTION ( 'NONE',  ( 1.000000000000000000, 0.000000000000000000, 0.000000000000000000 ) ) ;
#10819 = CYLINDRICAL_SURFACE ( 'NONE', #13842, 4.999999999999997335 ) ;
#10820 = CARTESIAN_POINT ( 'NONE',  ( 38.89115197531749857, 101.6687180808697377, 2.499999999999999556 ) ) ;
#10821 = AXIS2_PLACEMENT_3D ( 'NONE', #344, #4603, #13192 ) ;
#10822 = FACE_OUTER_BOUND ( 'NONE', #13358, .T. ) ;
#10823 = CARTESIAN_POINT ( 'NONE',  ( -9.175745902881725407E-17, 3.280056672672198914, -5.792110530374064999E-18 ) ) ;
#10824 = EDGE_CURVE ( 'NONE', #4918, #9172, #5263, .T. ) ;
#10825 = VERTEX_POINT ( 'NONE', #9505 ) ;
#10826 = VECTOR ( 'NONE', #2095, 1000.000000000000000 ) ;
#10827 = ORIENTED_EDGE ( 'NONE', *, *, #10786, .T. ) ;
#10828 = SURFACE_STYLE_USAGE ( .BOTH. , #11821 ) ;
#10829 = ORIENTED_EDGE ( 'NONE', *, *, #1729, .T. ) ;
#10830 = CARTESIAN_POINT ( 'NONE',  ( -1.077638310512993291E-15, 38.52236939141059935, -6.802498971006334016E-17 ) ) ;
#10831 = CARTESIAN_POINT ( 'NONE',  ( 8.385254915620292238, -3.520109059331727241, 1.035430912652128846E-15 ) ) ;
#10832 = AXIS2_PLACEMENT_3D ( 'NONE', #3601, #4580, #7885 ) ;
#10833 = DIRECTION ( 'NONE',  ( -6.158143864569485777E-17, -2.736152283717910599E-16, 1.000000000000000000 ) ) ;
#10834 = CARTESIAN_POINT ( 'NONE',  ( -8.385254915620295790, 12.70483462268160046, 16.77050983124058448 ) ) ;
#10835 = CIRCLE ( 'NONE', #9733, 2.000000000000003997 ) ;
#10836 = ORIENTED_EDGE ( 'NONE', *, *, #5567, .F. ) ;
#10837 = APPLICATION_CONTEXT ( 'automotive_design' ) ;
#10838 = ORIENTED_EDGE ( 'NONE', *, *, #2749, .F. ) ;
#10839 = DIRECTION ( 'NONE',  ( -1.000000000000000000, 0.000000000000000000, 0.000000000000000000 ) ) ;
#10840 = VECTOR ( 'NONE', #8698, 1000.000000000000000 ) ;
#10841 = ADVANCED_FACE ( 'NONE', ( #2067 ), #1021, .T. ) ;
#10842 = ORIENTED_EDGE ( 'NONE', *, *, #7059, .F. ) ;
#10843 = CARTESIAN_POINT ( 'NONE',  ( -35.04450421339218025, 112.5597086678580609, -2.499999999999998668 ) ) ;
#10844 = ORIENTED_EDGE ( 'NONE', *, *, #12901, .T. ) ;
#10845 = DIRECTION ( 'NONE',  ( -1.000000000000000000, -0.000000000000000000, -0.000000000000000000 ) ) ;
#10846 = LINE ( 'NONE', #9742, #10262 ) ;
#10847 = CARTESIAN_POINT ( 'NONE',  ( -1.087924057176452797, -78.56626508165413725, -10.04922990886309719 ) ) ;
#10848 = CARTESIAN_POINT ( 'NONE',  ( 40.56568360645881910, 100.7114851384503851, -1.410085254968634239 ) ) ;
#10849 = DIRECTION ( 'NONE',  ( -6.158143864569485777E-17, -2.736152283717910599E-16, 1.000000000000000000 ) ) ;
#10850 = FACE_OUTER_BOUND ( 'NONE', #3759, .T. ) ;
#10851 = AXIS2_PLACEMENT_3D ( 'NONE', #1416, #7868, #8846 ) ;
#10852 = ORIENTED_EDGE ( 'NONE', *, *, #2575, .F. ) ;
#10853 = ORIENTED_EDGE ( 'NONE', *, *, #4899, .F. ) ;
#10854 = VERTEX_POINT ( 'NONE', #1937 ) ;
#10855 = AXIS2_PLACEMENT_3D ( 'NONE', #6321, #6127, #860 ) ;
#10856 = ADVANCED_FACE ( 'NONE', ( #2000 ), #8990, .T. ) ;
#10857 = CARTESIAN_POINT ( 'NONE',  ( -4.267662252619976115, 91.33687515530510836, 2.605658972705547693 ) ) ;
#10858 = EDGE_CURVE ( 'NONE', #3017, #5860, #957, .T. ) ;
#10859 = CARTESIAN_POINT ( 'NONE',  ( -0.6169032162240980499, -80.00108109729535499, 10.04415339342917513 ) ) ;
#10860 = EDGE_LOOP ( 'NONE', ( #13321, #2850, #6342, #2764, #10381, #7552, #314, #7050, #12257, #11130, #11230, #3409, #5976, #2365, #6061, #11848, #4579, #7818, #12035, #11374, #10415, #3831, #242, #5453, #11975, #11154, #1842, #7594, #6751, #11992, #11061, #12491, #3886, #8806, #12280, #11333, #3144, #2782, #294, #5974, #13319, #12399, #5353, #1074, #4685, #7150, #1860, #9213, #10844, #10388, #9158, #12655, #5739, #1494, #3874, #13815, #8908, #4259, #4840, #5532, #2033, #13690 ) ) ;
#10861 = CARTESIAN_POINT ( 'NONE',  ( 34.99999999999958789, 1.063887963769481123E-13, 12.50000000000000000 ) ) ;
#10862 = CIRCLE ( 'NONE', #11769, 15.29705854078138927 ) ;
#10863 = CARTESIAN_POINT ( 'NONE',  ( 15.29705854078138927, 57.37192529142944863, -30.59411708156276788 ) ) ;
#10864 = CARTESIAN_POINT ( 'NONE',  ( 1.387778780781445676E-14, -100.0000000000000000, 0.000000000000000000 ) ) ;
#10865 = DIRECTION ( 'NONE',  ( 1.000000000000000000, -0.000000000000000000, 0.000000000000000000 ) ) ;
#10866 = EDGE_CURVE ( 'NONE', #9032, #11418, #12883, .T. ) ;
#10867 = DIRECTION ( 'NONE',  ( -6.158143864569485777E-17, -2.736152283717910599E-16, 1.000000000000000000 ) ) ;
#10868 = CARTESIAN_POINT ( 'NONE',  ( -10.14576398710722493, -69.00000000000014211, 0.5510781487875697771 ) ) ;
#10869 = CARTESIAN_POINT ( 'NONE',  ( -12.99553232110414491, -17.19957910547634228, -1.530749717005650972E-15 ) ) ;
#10870 = LINE ( 'NONE', #7720, #8374 ) ;
#10871 = ORIENTED_EDGE ( 'NONE', *, *, #1232, .F. ) ;
#10872 = CARTESIAN_POINT ( 'NONE',  ( 10.69346802281034847, 2.474956373702985601, 0.000000000000000000 ) ) ;
#10873 = CARTESIAN_POINT ( 'NONE',  ( 10.69381717166375623, 72.68333662216240043, -21.38763434332750535 ) ) ;
#10874 = ORIENTED_EDGE ( 'NONE', *, *, #269, .F. ) ;
#10875 = CARTESIAN_POINT ( 'NONE',  ( 15.29705854078138927, 90.00000000000000000, 1.714422261702872766E-15 ) ) ;
#10876 = CARTESIAN_POINT ( 'NONE',  ( -8.385254915620295790, -34.41905512736551032, 6.077912412602530076E-17 ) ) ;
#10877 = ADVANCED_FACE ( 'NONE', ( #12737 ), #7191, .T. ) ;
#10878 = CARTESIAN_POINT ( 'NONE',  ( -37.50000000000002132, 144.4948974278317735, 7.500000000000000000 ) ) ;
#10879 = ORIENTED_EDGE ( 'NONE', *, *, #7977, .F. ) ;
#10880 = DIRECTION ( 'NONE',  ( -0.7328050451781167318, -0.6804386568688601811, -2.409338161076489703E-16 ) ) ;
#10881 = ORIENTED_EDGE ( 'NONE', *, *, #13332, .F. ) ;
#10882 = CARTESIAN_POINT ( 'NONE',  ( 32.72727272727274084, 135.1423002281142089, -0.5000000000000000000 ) ) ;
#10883 = CARTESIAN_POINT ( 'NONE',  ( -12.99579180576517068, 26.38439787695498495, -1.684707622963446858E-15 ) ) ;
#10884 = AXIS2_PLACEMENT_3D ( 'NONE', #11951, #260, #6353 ) ;
#10885 = EDGE_CURVE ( 'NONE', #2631, #5397, #824, .T. ) ;
#10886 = CARTESIAN_POINT ( 'NONE',  ( 8.385254915620288685, 71.87811454074363837, 9.022884433393296612E-16 ) ) ;
#10887 = EDGE_CURVE ( 'NONE', #8407, #2160, #2811, .T. ) ;
#10888 = CARTESIAN_POINT ( 'NONE',  ( -15.29705854078139282, -1.063309978032473291, 1.877653204021102445E-18 ) ) ;
#10889 = CARTESIAN_POINT ( 'NONE',  ( 10.00000000000000711, 139.9999999999999716, -0.5000000000000000000 ) ) ;
#10890 = CARTESIAN_POINT ( 'NONE',  ( 12.99579180576517068, -30.16426982310158422, 25.99158361153035202 ) ) ;
#10891 = CYLINDRICAL_SURFACE ( 'NONE', #4996, 2.500000000000002220 ) ;
#10892 = CARTESIAN_POINT ( 'NONE',  ( 0.000000000000000000, 71.01020514433645303, 2.500000000000000000 ) ) ;
#10893 = ORIENTED_EDGE ( 'NONE', *, *, #1966, .T. ) ;
#10894 = EDGE_CURVE ( 'NONE', #9929, #5202, #1023, .T. ) ;
#10895 = ORIENTED_EDGE ( 'NONE', *, *, #4175, .F. ) ;
#10896 = DIRECTION ( 'NONE',  ( -1.000000000000000000, 0.000000000000000000, 0.000000000000000000 ) ) ;
#10897 = DIRECTION ( 'NONE',  ( 1.000000000000000000, 0.000000000000000000, 0.000000000000000000 ) ) ;
#10898 = ORIENTED_EDGE ( 'NONE', *, *, #10557, .T. ) ;
#10899 = DIRECTION ( 'NONE',  ( -2.797435172181481150E-17, 1.000000000000000000, -1.765856845898762549E-18 ) ) ;
#10900 = ADVANCED_FACE ( 'NONE', ( #3183 ), #13687, .T. ) ;
#10901 = VECTOR ( 'NONE', #13857, 1000.000000000000000 ) ;
#10902 = CARTESIAN_POINT ( 'NONE',  ( 25.00000000000001776, -99.15310334213020838, 0.4257687054510573832 ) ) ;
#10903 = DIRECTION ( 'NONE',  ( -6.158143864569485777E-17, -2.736152283717910599E-16, 1.000000000000000000 ) ) ;
#10904 = CARTESIAN_POINT ( 'NONE',  ( -10.69346802281034492, 11.89973432371241380, -1.351598593231734330E-15 ) ) ;
#10905 = ORIENTED_EDGE ( 'NONE', *, *, #6941, .F. ) ;
#10906 = VERTEX_POINT ( 'NONE', #9641 ) ;
#10907 = ORIENTED_EDGE ( 'NONE', *, *, #7724, .F. ) ;
#10908 = FACE_OUTER_BOUND ( 'NONE', #2763, .T. ) ;
#10909 = EDGE_LOOP ( 'NONE', ( #8053, #9177, #10247, #3689 ) ) ;
#10910 = CARTESIAN_POINT ( 'NONE',  ( 12.99579180576516713, 73.50828762700209040, 3.183050967463143379E-15 ) ) ;
#10911 = AXIS2_PLACEMENT_3D ( 'NONE', #530, #12151, #5767 ) ;
#10912 = DIRECTION ( 'NONE',  ( -2.797435172181481150E-17, 1.000000000000000000, -1.765856845898762549E-18 ) ) ;
#10913 = CARTESIAN_POINT ( 'NONE',  ( 18.44105126153190710, 8.793532718851093222, 2.500000000000001332 ) ) ;
#10914 = B_SPLINE_CURVE_WITH_KNOTS ( 'NONE', 3,
 ( #12739, #3116, #13320, #6554 ),
 .UNSPECIFIED., .F., .F.,
 ( 4, 4 ),
 ( 0.000000000000000000, 1.000000000000000000 ),
 .UNSPECIFIED. ) ;
#10915 = CIRCLE ( 'NONE', #7342, 25.50000000002550138 ) ;
#10916 = LINE ( 'NONE', #13211, #9988 ) ;
#10917 = DIRECTION ( 'NONE',  ( -6.158143864569485777E-17, -2.736152283717910599E-16, 1.000000000000000000 ) ) ;
#10918 = CARTESIAN_POINT ( 'NONE',  ( -8.620861567158451422, -92.33329736102577101, 0.6435148816328051247 ) ) ;
#10919 = DIRECTION ( 'NONE',  ( -0.4226182617407014397, 0.9063077870366489375, 0.000000000000000000 ) ) ;
#10920 = VERTEX_POINT ( 'NONE', #5155 ) ;
#10921 = VERTEX_POINT ( 'NONE', #10680 ) ;
#10922 = EDGE_LOOP ( 'NONE', ( #10708, #12709, #7618, #8962 ) ) ;
#10923 = B_SPLINE_CURVE_WITH_KNOTS ( 'NONE', 3,
 ( #11964, #2355, #274, #7908 ),
 .UNSPECIFIED., .F., .F.,
 ( 4, 4 ),
 ( 0.000000000000000000, 1.000000000000000000 ),
 .UNSPECIFIED. ) ;
#10924 = AXIS2_PLACEMENT_3D ( 'NONE', #1525, #11211, #9109 ) ;
#10925 = DIRECTION ( 'NONE',  ( 0.9960067511297464593, -0.08927794634716622324, 3.401418580343279473E-17 ) ) ;
#10926 = AXIS2_PLACEMENT_3D ( 'NONE', #8386, #3058, #4169 ) ;
#10927 = DIRECTION ( 'NONE',  ( 1.000000000000000000, 0.000000000000000000, 0.000000000000000000 ) ) ;
#10928 =( BOUNDED_SURFACE ( )  B_SPLINE_SURFACE ( 3, 3, ( 
 ( #4349, #6664, #3299, #7714 ),
 ( #4494, #1334, #3233, #7578 ),
 ( #6539, #7651, #12797, #11792 ),
 ( #5475, #11858, #13081, #11724 ) ),
 .UNSPECIFIED., .F., .F., .T. ) 
 B_SPLINE_SURFACE_WITH_KNOTS ( ( 4, 4 ),
 ( 4, 4 ),
 ( 0.000000000000000000, 1.000000000000000000 ),
 ( 0.000000000000000000, 1.000000000000000000 ),
 .UNSPECIFIED. ) 
 GEOMETRIC_REPRESENTATION_ITEM ( )  RATIONAL_B_SPLINE_SURFACE ( (
 ( 1.000000000000000000, 0.3333333333333334259, 0.3333333333333334259, 1.000000000000000000),
 ( 1.000000000000000000, 0.3333333333333334259, 0.3333333333333334259, 1.000000000000000000),
 ( 1.000000000000000000, 0.3333333333333334259, 0.3333333333333334259, 1.000000000000000000),
 ( 1.000000000000000000, 0.3333333333333334259, 0.3333333333333334259, 1.000000000000000000) ) ) 
 REPRESENTATION_ITEM ( '' )  SURFACE ( )  );
#10929 = ORIENTED_EDGE ( 'NONE', *, *, #704, .T. ) ;
#10930 = DIRECTION ( 'NONE',  ( 0.000000000000000000, 0.000000000000000000, 1.000000000000000000 ) ) ;
#10931 = DIRECTION ( 'NONE',  ( 0.000000000000000000, 0.000000000000000000, 1.000000000000000000 ) ) ;
#10932 = CARTESIAN_POINT ( 'NONE',  ( -10.69381717166375623, 34.98422482212468054, -1.433169162795722386E-15 ) ) ;
#10933 = CARTESIAN_POINT ( 'NONE',  ( 25.00000000000001421, -34.99999999999999289, -7.500000000000000000 ) ) ;
#10934 = CARTESIAN_POINT ( 'NONE',  ( -0.2714810715539830999, -148.3982683978709929, -1.717521498780891109 ) ) ;
#10935 = CARTESIAN_POINT ( 'NONE',  ( -15.29705854078139637, 0.8232575913728885642, -1.453755053663958216E-18 ) ) ;
#10936 = DIRECTION ( 'NONE',  ( 1.000000000000000000, 0.000000000000000000, 0.000000000000000000 ) ) ;
#10937 = CARTESIAN_POINT ( 'NONE',  ( -6.374260517225369682, -76.81818181818198354, -7.989319691426040926 ) ) ;
#10938 = AXIS2_PLACEMENT_3D ( 'NONE', #8798, #12177, #7895 ) ;
#10939 = DIRECTION ( 'NONE',  ( 0.9556796851544553384, -0.2944084567112177364, -2.313087999326726136E-17 ) ) ;
#10940 = DIRECTION ( 'NONE',  ( 0.000000000000000000, 0.000000000000000000, 1.000000000000000000 ) ) ;
#10941 = EDGE_CURVE ( 'NONE', #5403, #7000, #6377, .T. ) ;
#10942 = VERTEX_POINT ( 'NONE', #11472 ) ;
#10943 = VERTEX_POINT ( 'NONE', #13752 ) ;
#10944 = CARTESIAN_POINT ( 'NONE',  ( 16.29599561779310335, 1.298160649189404880, -2.500000000000000000 ) ) ;
#10945 = ORIENTED_EDGE ( 'NONE', *, *, #13603, .F. ) ;
#10946 = CARTESIAN_POINT ( 'NONE',  ( 10.00000000000000000, 99.99999999999994316, -0.5000000000000000000 ) ) ;
#10947 = AXIS2_PLACEMENT_3D ( 'NONE', #1505, #6069, #7962 ) ;
#10948 = DIRECTION ( 'NONE',  ( -6.158143864569485777E-17, -2.736152283717910599E-16, 1.000000000000000000 ) ) ;
#10949 = ORIENTED_EDGE ( 'NONE', *, *, #1465, .F. ) ;
#10950 = ORIENTED_EDGE ( 'NONE', *, *, #13430, .T. ) ;
#10951 = CARTESIAN_POINT ( 'NONE',  ( -1.673669778670227307E-15, 59.82872437272870769, -1.056489625149731375E-16 ) ) ;
#10952 = ORIENTED_EDGE ( 'NONE', *, *, #5568, .T. ) ;
#10953 = CARTESIAN_POINT ( 'NONE',  ( -23.75056915604791641, -98.97863401284405427, -7.500000000000000000 ) ) ;
#10954 = CIRCLE ( 'NONE', #684, 16.99999999999998934 ) ;
#10955 = CIRCLE ( 'NONE', #11635, 40.00000000000001421 ) ;
#10956 = DIRECTION ( 'NONE',  ( 0.000000000000000000, -1.000000000000000000, 0.000000000000000000 ) ) ;
#10957 = DIRECTION ( 'NONE',  ( -1.000000000000000000, 0.000000000000000000, 0.000000000000000000 ) ) ;
#10958 = CARTESIAN_POINT ( 'NONE',  ( -35.00000000000000000, -4.286263797015736496E-15, -8.499999999999998224 ) ) ;
#10959 = CARTESIAN_POINT ( 'NONE',  ( -35.00000000000000000, -4.286263797015736496E-15, 8.499999999999998224 ) ) ;
#10960 = CARTESIAN_POINT ( 'NONE',  ( -8.385254915620292238, -31.79444290936001138, 5.614443467303076398E-17 ) ) ;
#10961 = FACE_OUTER_BOUND ( 'NONE', #7072, .T. ) ;
#10962 = DIRECTION ( 'NONE',  ( 6.158143864569485777E-17, 2.736152283717910599E-16, -1.000000000000000000 ) ) ;
#10963 = EDGE_CURVE ( 'NONE', #2483, #4263, #6152, .T. ) ;
#10964 = DIRECTION ( 'NONE',  ( -1.000000000000000000, 0.000000000000000000, 0.000000000000000000 ) ) ;
#10965 = CIRCLE ( 'NONE', #13016, 2.000000000000003997 ) ;
#10966 = ORIENTED_EDGE ( 'NONE', *, *, #3842, .T. ) ;
#10967 = FACE_OUTER_BOUND ( 'NONE', #3547, .T. ) ;
#10968 = CIRCLE ( 'NONE', #4942, 15.29705854078138749 ) ;
#10969 = ORIENTED_EDGE ( 'NONE', *, *, #1118, .T. ) ;
#10970 = EDGE_CURVE ( 'NONE', #12412, #470, #13370, .T. ) ;
#10971 = EDGE_CURVE ( 'NONE', #10943, #9931, #113, .T. ) ;
#10972 = ORIENTED_EDGE ( 'NONE', *, *, #7805, .T. ) ;
#10973 = DIRECTION ( 'NONE',  ( 0.9960067511297463483, -0.08927794634716618161, 4.818676322152979407E-17 ) ) ;
#10974 = CIRCLE ( 'NONE', #4725, 15.70031846811053455 ) ;
#10975 = ITEM_DEFINED_TRANSFORMATION ( 'NONE', 'NONE', #5067,  #8193 ) ;
#10976 = ORIENTED_EDGE ( 'NONE', *, *, #13080, .T. ) ;
#10977 = FACE_OUTER_BOUND ( 'NONE', #3991, .T. ) ;
#10978 = AXIS2_PLACEMENT_3D ( 'NONE', #7039, #7952, #2900 ) ;
#10979 = CARTESIAN_POINT ( 'NONE',  ( 15.29705854078139282, 64.91013567203349055, 1.757061666260241085E-15 ) ) ;
#10980 = FACE_OUTER_BOUND ( 'NONE', #4131, .T. ) ;
#10981 = CARTESIAN_POINT ( 'NONE',  ( -15.29705854078139282, 90.00000000000000000, -1.589271161308885878E-16 ) ) ;
#10982 = CARTESIAN_POINT ( 'NONE',  ( 34.99999999999999289, 25.00000000000002132, 7.500000000000000000 ) ) ;
#10983 = ORIENTED_EDGE ( 'NONE', *, *, #3161, .T. ) ;
#10984 = CIRCLE ( 'NONE', #3146, 8.385254915620290461 ) ;
#10985 = ORIENTED_EDGE ( 'NONE', *, *, #13589, .F. ) ;
#10986 = EDGE_CURVE ( 'NONE', #6682, #7192, #9912, .T. ) ;
#10987 = EDGE_LOOP ( 'NONE', ( #2360, #10644, #4593, #838 ) ) ;
#10988 = ORIENTED_EDGE ( 'NONE', *, *, #5070, .T. ) ;
#10989 = ORIENTED_EDGE ( 'NONE', *, *, #8245, .F. ) ;
#10990 = ORIENTED_EDGE ( 'NONE', *, *, #1386, .F. ) ;
#10991 = CARTESIAN_POINT ( 'NONE',  ( -12.99553232110414491, -26.62435705548577047, -1.497464099677451275E-15 ) ) ;
#10992 = CARTESIAN_POINT ( 'NONE',  ( 35.00000000000000000, -4.286263797015736496E-15, -4.000000000000000000 ) ) ;
#10993 = CARTESIAN_POINT ( 'NONE',  ( -8.385254915620292238, 34.17900274070598243, -6.035522597566817733E-17 ) ) ;
#10994 = AXIS2_PLACEMENT_3D ( 'NONE', #11117, #4810, #9226 ) ;
#10995 = CARTESIAN_POINT ( 'NONE',  ( -34.26147919318643886, 108.1862277804541321, 0.7448039452652762682 ) ) ;
#10996 = LINE ( 'NONE', #5679, #12855 ) ;
#10997 = CARTESIAN_POINT ( 'NONE',  ( -5.855857762045447501, -86.34391607673575209, 7.325803626397927815 ) ) ;
#10998 = LINE ( 'NONE', #7314, #370 ) ;
#10999 = ORIENTED_EDGE ( 'NONE', *, *, #4289, .F. ) ;
#11000 = ORIENTED_EDGE ( 'NONE', *, *, #2830, .F. ) ;
#11001 = ORIENTED_EDGE ( 'NONE', *, *, #13689, .F. ) ;
#11002 = EDGE_CURVE ( 'NONE', #8545, #6810, #3920, .T. ) ;
#11003 = VERTEX_POINT ( 'NONE', #10748 ) ;
#11004 = CIRCLE ( 'NONE', #1835, 18.74900000001875355 ) ;
#11005 = CYLINDRICAL_SURFACE ( 'NONE', #2001, 2.000000000000001776 ) ;
#11006 = EDGE_CURVE ( 'NONE', #11917, #8407, #7275, .T. ) ;
#11007 = CARTESIAN_POINT ( 'NONE',  ( 22.00707094244967621, -21.94159963418280057, 2.499999999999992895 ) ) ;
#11008 = ORIENTED_EDGE ( 'NONE', *, *, #3203, .T. ) ;
#11009 = CARTESIAN_POINT ( 'NONE',  ( 76.84607712649204814, -99.92541302764922762, 2.500000000000000000 ) ) ;
#11010 = CARTESIAN_POINT ( 'NONE',  ( -8.385254915620294014, 59.82872437272870769, -2.210471567782421984E-15 ) ) ;
#11011 = DIRECTION ( 'NONE',  ( -6.158143864569485777E-17, -2.736152283717910599E-16, 1.000000000000000000 ) ) ;
#11012 = CARTESIAN_POINT ( 'NONE',  ( 2.054569550993968541, -122.9090909090962924, 4.917417506341301703 ) ) ;
#11013 = CARTESIAN_POINT ( 'NONE',  ( -10.69381717166375623, 44.40900277213413716, -1.466454780123922280E-15 ) ) ;
#11014 = CARTESIAN_POINT ( 'NONE',  ( 23.44929957547844879, 14.76842309468663750, -2.499999999999996447 ) ) ;
#11015 = CARTESIAN_POINT ( 'NONE',  ( 2.134167523386926835, -102.5454545454519746, 7.554873526039220799 ) ) ;
#11016 = CYLINDRICAL_SURFACE ( 'NONE', #13383, 31.93204061526060045 ) ;
#11017 = DIRECTION ( 'NONE',  ( -0.000000000000000000, -0.000000000000000000, -1.000000000000000000 ) ) ;
#11018 = DIRECTION ( 'NONE',  ( -6.158143864569485777E-17, -2.736152283717910599E-16, 1.000000000000000000 ) ) ;
#11019 = VERTEX_POINT ( 'NONE', #319 ) ;
#11020 = ORIENTED_EDGE ( 'NONE', *, *, #723, .T. ) ;
#11021 = ORIENTED_EDGE ( 'NONE', *, *, #1041, .F. ) ;
#11022 = DIRECTION ( 'NONE',  ( 0.7533101279583153120, -0.6576654553155628635, -1.445602896645893822E-16 ) ) ;
#11023 = CARTESIAN_POINT ( 'NONE',  ( 40.00000000000000711, 100.0000000000000000, 2.500000000000000000 ) ) ;
#11024 = CARTESIAN_POINT ( 'NONE',  ( -24.99999999999998934, -99.29838587104467251, -2.138129719433996545 ) ) ;
#11025 = CIRCLE ( 'NONE', #4314, 8.385254915620295790 ) ;
#11026 = DIRECTION ( 'NONE',  ( -2.797435172181481150E-17, 1.000000000000000000, -1.765856845898762549E-18 ) ) ;
#11027 = ORIENTED_EDGE ( 'NONE', *, *, #11246, .T. ) ;
#11028 = AXIS2_PLACEMENT_3D ( 'NONE', #3607, #7893, #12175 ) ;
#11029 = ORIENTED_EDGE ( 'NONE', *, *, #11692, .F. ) ;
#11030 = DIRECTION ( 'NONE',  ( -0.000000000000000000, -1.000000000000000000, -0.000000000000000000 ) ) ;
#11031 = EDGE_LOOP ( 'NONE', ( #1255, #13312, #12439, #5246 ) ) ;
#11032 = CARTESIAN_POINT ( 'NONE',  ( 15.29705854078139282, 64.91013567203349055, 1.757061666260241085E-15 ) ) ;
#11033 = ADVANCED_FACE ( 'NONE', ( #1224 ), #6614, .T. ) ;
#11034 = CARTESIAN_POINT ( 'NONE',  ( -12.99579180576517068, 54.65873172698324112, -1.784564474948045950E-15 ) ) ;
#11035 = CARTESIAN_POINT ( 'NONE',  ( 34.31346379765670918, 108.0181378390413016, -1.328939170454190855 ) ) ;
#11036 = DIRECTION ( 'NONE',  ( -0.8000000000000010436, 0.5999999999999985345, 0.000000000000000000 ) ) ;
#11037 = CARTESIAN_POINT ( 'NONE',  ( -12.99579180576517423, -30.16426982310158067, -1.484993918994249462E-15 ) ) ;
#11038 = DIRECTION ( 'NONE',  ( 1.000000000000000000, -1.665334536937735599E-15, 0.000000000000000000 ) ) ;
#11039 = CARTESIAN_POINT ( 'NONE',  ( 8.385254915620292238, -22.36966495935058319, 1.068716529980328346E-15 ) ) ;
#11040 = FACE_OUTER_BOUND ( 'NONE', #8555, .T. ) ;
#11041 = VECTOR ( 'NONE', #929, 1000.000000000000000 ) ;
#11042 = CARTESIAN_POINT ( 'NONE',  ( -6.924833908958124424E-16, 24.75422479069652582, -4.371241731156832241E-17 ) ) ;
#11043 = AXIS2_PLACEMENT_3D ( 'NONE', #123, #5560, #5425 ) ;
#11044 = DIRECTION ( 'NONE',  ( 0.000000000000000000, -1.000000000000000000, 0.000000000000000000 ) ) ;
#11045 = CARTESIAN_POINT ( 'NONE',  ( 4.131580040049976255, 90.90692022676346085, 2.817507346490923048 ) ) ;
#11046 = VERTEX_POINT ( 'NONE', #10876 ) ;
#11047 = EDGE_LOOP ( 'NONE', ( #8706, #11139, #2526, #2894, #12625, #11574, #10020, #7225, #9073, #1288, #5646, #3399 ) ) ;
#11048 = AXIS2_PLACEMENT_3D ( 'NONE', #8507, #12526, #5213 ) ;
#11049 = FACE_OUTER_BOUND ( 'NONE', #6397, .T. ) ;
#11050 = ADVANCED_FACE ( 'NONE', ( #6679 ), #4365, .T. ) ;
#11051 = APPLICATION_PROTOCOL_DEFINITION ( 'draft international standard', 'automotive_design', 1998, #3147 ) ;
#11052 = EDGE_CURVE ( 'NONE', #3832, #182, #8401, .T. ) ;
#11053 = VERTEX_POINT ( 'NONE', #8648 ) ;
#11054 = LINE ( 'NONE', #4388, #7704 ) ;
#11055 = CARTESIAN_POINT ( 'NONE',  ( -39.06230589874905235, 109.5835921350012825, 7.500000000000000000 ) ) ;
#11056 = EDGE_CURVE ( 'NONE', #5338, #6314, #795, .T. ) ;
#11057 = EDGE_CURVE ( 'NONE', #13719, #2222, #7661, .T. ) ;
#11058 = CARTESIAN_POINT ( 'NONE',  ( -8.385254915620294014, 22.12961257269105531, -1.105053014962047635E-15 ) ) ;
#11059 = CARTESIAN_POINT ( 'NONE',  ( 10.10544246783441835, -70.44230941463432316, 0.3214603529571786189 ) ) ;
#11060 = CIRCLE ( 'NONE', #12415, 72.49999999999998579 ) ;
#11061 = ORIENTED_EDGE ( 'NONE', *, *, #1816, .T. ) ;
#11062 = ORIENTED_EDGE ( 'NONE', *, *, #11901, .F. ) ;
#11063 = AXIS2_PLACEMENT_3D ( 'NONE', #12692, #7276, #7480 ) ;
#11064 = EDGE_CURVE ( 'NONE', #2246, #6588, #7930, .T. ) ;
#11065 = ORIENTED_EDGE ( 'NONE', *, *, #9008, .F. ) ;
#11066 = ORIENTED_EDGE ( 'NONE', *, *, #8493, .F. ) ;
#11067 = EDGE_CURVE ( 'NONE', #7956, #2525, #11320, .T. ) ;
#11068 = ORIENTED_EDGE ( 'NONE', *, *, #7758, .F. ) ;
#11069 = CARTESIAN_POINT ( 'NONE',  ( -15.29705854078139460, -27.45107625865536605, 4.847467093863555185E-17 ) ) ;
#11070 = AXIS2_PLACEMENT_3D ( 'NONE', #5293, #1094, #2198 ) ;
#11071 = LINE ( 'NONE', #13361, #12043 ) ;
#11072 = AXIS2_PLACEMENT_3D ( 'NONE', #12598, #7112, #6141 ) ;
#11073 = EDGE_CURVE ( 'NONE', #5183, #10278, #3235, .T. ) ;
#11074 = CARTESIAN_POINT ( 'NONE',  ( 25.00000000000000355, 120.0000000000000142, 2.499999999999999556 ) ) ;
#11075 = EDGE_CURVE ( 'NONE', #5607, #4393, #2580, .T. ) ;
#11076 = CARTESIAN_POINT ( 'NONE',  ( 25.00000000000000355, 120.0000000000000284, 0.5000000000000000000 ) ) ;
#11077 = LINE ( 'NONE', #1469, #9259 ) ;
#11078 = CARTESIAN_POINT ( 'NONE',  ( -15.29705854078139105, 57.37192529142945574, -2.075970591910287010E-15 ) ) ;
#11079 = VERTEX_POINT ( 'NONE', #10809 ) ;
#11080 = ORIENTED_EDGE ( 'NONE', *, *, #3976, .F. ) ;
#11081 = VERTEX_POINT ( 'NONE', #12083 ) ;
#11082 = AXIS2_PLACEMENT_3D ( 'NONE', #2195, #9840, #6550 ) ;
#11083 = AXIS2_PLACEMENT_3D ( 'NONE', #3887, #10134, #8166 ) ;
#11084 = CARTESIAN_POINT ( 'NONE',  ( 10.69346802281034314, -25.79937747632526879, 21.38693604562069694 ) ) ;
#11085 = CARTESIAN_POINT ( 'NONE',  ( 4.250272934615505704, -76.81818181818026403, 9.136824450690475885 ) ) ;
#11086 = ORIENTED_EDGE ( 'NONE', *, *, #10476, .T. ) ;
#11087 = CARTESIAN_POINT ( 'NONE',  ( -2.517691654963332357E-15, 90.00000000000000000, -1.589271161308885878E-16 ) ) ;
#11088 = DIRECTION ( 'NONE',  ( 1.000000000000000000, 0.000000000000000000, 0.000000000000000000 ) ) ;
#11089 = FACE_OUTER_BOUND ( 'NONE', #4469, .T. ) ;
#11090 = CARTESIAN_POINT ( 'NONE',  ( 0.1852016367018599896, -70.00000000000000000, -1.488522876466113809 ) ) ;
#11091 = AXIS2_PLACEMENT_3D ( 'NONE', #2698, #11380, #6974 ) ;
#11092 = CARTESIAN_POINT ( 'NONE',  ( 5.655105406253481348, -85.78354978357639027, -8.815184813446974132 ) ) ;
#11093 = EDGE_CURVE ( 'NONE', #4208, #5686, #1916, .T. ) ;
#11094 = DIRECTION ( 'NONE',  ( 1.000000000000000000, 0.000000000000000000, 0.000000000000000000 ) ) ;
#11095 = CARTESIAN_POINT ( 'NONE',  ( -2.517691654963332357E-15, 90.00000000000000000, -1.589271161308885878E-16 ) ) ;
#11096 = DIRECTION ( 'NONE',  ( 1.000000000000000000, 0.000000000000000000, 0.000000000000000000 ) ) ;
#11097 = PRESENTATION_LAYER_ASSIGNMENT (  '', '', ( #3700 ) ) ;
#11098 = DIRECTION ( 'NONE',  ( 0.000000000000000000, 0.000000000000000000, 1.000000000000000000 ) ) ;
#11099 = CIRCLE ( 'NONE', #2131, 21.99999999999999289 ) ;
#11100 = ORIENTED_EDGE ( 'NONE', *, *, #13462, .F. ) ;
#11101 = ORIENTED_EDGE ( 'NONE', *, *, #3955, .F. ) ;
#11102 = ORIENTED_EDGE ( 'NONE', *, *, #11246, .F. ) ;
#11103 = CYLINDRICAL_SURFACE ( 'NONE', #4962, 15.00000000000000000 ) ;
#11104 = ORIENTED_EDGE ( 'NONE', *, *, #9011, .F. ) ;
#11105 = CARTESIAN_POINT ( 'NONE',  ( -3.377085873584029674, -129.6408637431290458, 2.289279048948418716 ) ) ;
#11106 = DIRECTION ( 'NONE',  ( 0.9960067511297464593, -0.08927794634716622324, 6.802837160686558945E-17 ) ) ;
#11107 = CARTESIAN_POINT ( 'NONE',  ( 35.20000000000002416, 106.4000000000000057, 2.500000000000000000 ) ) ;
#11108 = VECTOR ( 'NONE', #582, 1000.000000000000000 ) ;
#11109 = LINE ( 'NONE', #13315, #805 ) ;
#11110 = CARTESIAN_POINT ( 'NONE',  ( 2.179449471770333435, 90.00000000000000000, -4.500000000000000888 ) ) ;
#11111 = ORIENTED_EDGE ( 'NONE', *, *, #9297, .F. ) ;
#11112 = ORIENTED_EDGE ( 'NONE', *, *, #10054, .T. ) ;
#11113 = DIRECTION ( 'NONE',  ( -2.797435172181481150E-17, 1.000000000000000000, -1.765856845898762549E-18 ) ) ;
#11114 = ORIENTED_EDGE ( 'NONE', *, *, #13865, .T. ) ;
#11115 = AXIS2_PLACEMENT_3D ( 'NONE', #5024, #2921, #4884 ) ;
#11116 = CARTESIAN_POINT ( 'NONE',  ( -31.81818181818181657, 133.3608531424536920, -0.5000000000000000000 ) ) ;
#11117 = CARTESIAN_POINT ( 'NONE',  ( 0.000000000000000000, 71.01020514433645303, -7.500000000000000000 ) ) ;
#11118 = DIRECTION ( 'NONE',  ( 0.000000000000000000, 0.000000000000000000, 1.000000000000000000 ) ) ;
#11119 = DIRECTION ( 'NONE',  ( 2.797435172181480534E-17, -1.000000000000000000, 1.765856845898762164E-18 ) ) ;
#11120 = CARTESIAN_POINT ( 'NONE',  ( -2.008006351130390499, -80.00378950643924725, -9.910921267331605833 ) ) ;
#11121 = CARTESIAN_POINT ( 'NONE',  ( 25.00000000000000355, 120.0000000000000142, 7.500000000000000000 ) ) ;
#11122 = AXIS2_PLACEMENT_3D ( 'NONE', #3326, #3259, #9788 ) ;
#11123 = DIRECTION ( 'NONE',  ( -2.797435172181481150E-17, 1.000000000000000000, -1.765856845898762549E-18 ) ) ;
#11124 = B_SPLINE_CURVE_WITH_KNOTS ( 'NONE', 3,
 ( #7178, #5080, #12451, #11662, #1080, #3371, #5540, #13085, #12802, #3169 ),
 .UNSPECIFIED., .F., .F.,
 ( 4, 3, 3, 4 ),
 ( 0.000000000000000000, 0.0006882994548164135529, 0.001843858713197575735, 0.002999417971958379548 ),
 .UNSPECIFIED. ) ;
#11125 = CARTESIAN_POINT ( 'NONE',  ( -10.69346802281034314, -6.949821576306441706, -21.38693604562069694 ) ) ;
#11126 = CARTESIAN_POINT ( 'NONE',  ( -10.69381717166375267, 53.83378072214353693, -21.38763434332751245 ) ) ;
#11127 = ORIENTED_EDGE ( 'NONE', *, *, #5654, .F. ) ;
#11128 = CARTESIAN_POINT ( 'NONE',  ( 56.97938482224745371, -167.3636363686644870, 8.923382219704807383 ) ) ;
#11129 = AXIS2_PLACEMENT_3D ( 'NONE', #12117, #12261, #4761 ) ;
#11130 = ORIENTED_EDGE ( 'NONE', *, *, #11067, .T. ) ;
#11131 = LINE ( 'NONE', #8804, #6154 ) ;
#11132 = ITEM_DEFINED_TRANSFORMATION ( 'NONE', 'NONE', #4605,  #8193 ) ;
#11133 = EDGE_LOOP ( 'NONE', ( #6868, #4516, #10050, #12902, #6428, #3331 ) ) ;
#11134 = CARTESIAN_POINT ( 'NONE',  ( -10.69381717166375090, 34.98422482212468054, -21.38763434332750890 ) ) ;
#11135 = CARTESIAN_POINT ( 'NONE',  ( 8.207015671355002297E-16, -29.33764382806072746, 5.180607919632063331E-17 ) ) ;
#11136 = FACE_OUTER_BOUND ( 'NONE', #8916, .T. ) ;
#11137 = DIRECTION ( 'NONE',  ( 1.000000000000000000, 0.000000000000000000, 0.000000000000000000 ) ) ;
#11138 = CARTESIAN_POINT ( 'NONE',  ( 15.29705854078138749, -38.76242177807012723, 30.59411708156277854 ) ) ;
#11139 = ORIENTED_EDGE ( 'NONE', *, *, #719, .F. ) ;
#11140 = B_SPLINE_SURFACE_WITH_KNOTS ( 'NONE', 3, 3, ( 
 ( #6911, #11128, #5880, #8114, #7052, #5797, #11198, #8178, #10150, #3758, #4954, #12463, #10217, #13412, #2715, #9096, #555, #12179, #6991, #11331, #6012, #13484, #10353, #13338 ),
 ( #6849, #8042, #3830, #10281, #1515, #3687, #4820, #10076, #488, #13549, #9236, #2642, #2846, #12323, #5944, #683, #9027, #621, #7973, #12254, #4881, #12397, #11395, #753 ),
 ( #5019, #3969, #9442, #12605, #7254, #13880, #6345, #7387, #9301, #7320, #13750, #10612, #1933, #8378, #10417, #2916, #10481, #1998, #2125, #6150, #6220, #11469, #1020, #4227 ),
 ( #3112, #7456, #13620, #954, #6278, #4096, #13683, #2982, #8242, #10550, #9371, #883, #5151, #5216, #9503, #9569, #13813, #4163, #8447, #12734, #5288, #12815, #11737, #12534 ) ),
 .UNSPECIFIED., .F., .F., .F.,
 ( 4, 4 ),
 ( 4, 1, 1, 1, 1, 1, 1, 1, 1, 1, 1, 1, 1, 1, 1, 1, 1, 1, 1, 1, 1, 4 ),
 ( -0.02200000000000000566, 0.002000000000000001776 ),
 ( -0.009000000000000030545, -0.004090909090909119854, -2.775557561562891043E-17, 0.0008181818181817908375, 0.005727272727272700661, 0.01250649350649347610, 0.02045454545454543360, 0.02536363636363634516, 0.03027272727272725672, 0.03518181818181816828, 0.04009090909090907984, 0.04990909090909089602, 0.05481818181818180757, 0.05972727272727271913, 0.06463636363636363069, 0.06954545454545453531, 0.07749350649350648934, 0.08427272727272726305, 0.08918181818181818155, 0.08999999999999998279, 0.09409090909090908617, 0.09900000000000000466 ),
 .UNSPECIFIED. ) ;
#11141 = ADVANCED_FACE ( 'NONE', ( #8784 ), #13018, .T. ) ;
#11142 = ORIENTED_EDGE ( 'NONE', *, *, #1652, .T. ) ;
#11143 = EDGE_CURVE ( 'NONE', #6441, #11311, #9272, .T. ) ;
#11144 = CARTESIAN_POINT ( 'NONE',  ( 2.008006476061143353, -80.00378950643523979, 9.910921260988354575 ) ) ;
#11145 = PRODUCT_DEFINITION ( 'UNKNOWN', '', #13137, #2510 ) ;
#11146 = VERTEX_POINT ( 'NONE', #10946 ) ;
#11147 = VERTEX_POINT ( 'NONE', #10198 ) ;
#11148 = DIRECTION ( 'NONE',  ( 1.000000000000000000, -0.000000000000000000, -0.000000000000000000 ) ) ;
#11149 = CARTESIAN_POINT ( 'NONE',  ( -25.00000000000000355, 120.0000000000000284, 2.500000000000000000 ) ) ;
#11150 = CARTESIAN_POINT ( 'NONE',  ( 18.99432778721693893, 26.96223687785628442, 6.295342420724995058 ) ) ;
#11151 = CARTESIAN_POINT ( 'NONE',  ( 8.385254915620299343, -34.41905512736551032, 1.085359338644428786E-15 ) ) ;
#11152 = CARTESIAN_POINT ( 'NONE',  ( 8.592794974440716160, -91.93698159008127391, -1.116928117929663955 ) ) ;
#11153 = CARTESIAN_POINT ( 'NONE',  ( -15.29705854078139282, 57.37192529142944863, 30.59411708156276788 ) ) ;
#11154 = ORIENTED_EDGE ( 'NONE', *, *, #1279, .F. ) ;
#11155 = EDGE_CURVE ( 'NONE', #8094, #5991, #12445, .T. ) ;
#11156 = EDGE_LOOP ( 'NONE', ( #1344, #12029, #13622, #10969 ) ) ;
#11157 = ADVANCED_FACE ( 'NONE', ( #5004 ), #7069, .T. ) ;
#11158 = EDGE_CURVE ( 'NONE', #10350, #214, #10646, .T. ) ;
#11159 = DIRECTION ( 'NONE',  ( 0.000000000000000000, 0.000000000000000000, 1.000000000000000000 ) ) ;
#11160 = CIRCLE ( 'NONE', #10035, 2.500000000000002220 ) ;
#11161 = CARTESIAN_POINT ( 'NONE',  ( 5.783440176334763372, -75.54545454545555572, 8.231660884606897710 ) ) ;
#11162 = ORIENTED_EDGE ( 'NONE', *, *, #11901, .T. ) ;
#11163 = CARTESIAN_POINT ( 'NONE',  ( 39.99999999999999289, 120.0000000000000284, -0.5000000000000000000 ) ) ;
#11164 =( NAMED_UNIT ( * ) PLANE_ANGLE_UNIT ( ) SI_UNIT ( $, .RADIAN. ) );
#11165 = CARTESIAN_POINT ( 'NONE',  ( 15.29705854078139105, -10.48808792804187284, 1.890204135573039875E-15 ) ) ;
#11166 = DIRECTION ( 'NONE',  ( 0.9923485843107423543, 2.797833471351478217E-17, 0.1234677578012386562 ) ) ;
#11167 = CARTESIAN_POINT ( 'NONE',  ( -3.371721678969553881, -122.9090909090926260, -4.477688567679849463 ) ) ;
#11168 = DIRECTION ( 'NONE',  ( 0.000000000000000000, 0.000000000000000000, 1.000000000000000000 ) ) ;
#11169 = CARTESIAN_POINT ( 'NONE',  ( 15.65588872828332612, -16.61546069029112260, -1.359866191199148089 ) ) ;
#11170 = CARTESIAN_POINT ( 'NONE',  ( -19.18070798040252711, 20.00000000000000000, -4.000000000000000000 ) ) ;
#11171 = ORIENTED_EDGE ( 'NONE', *, *, #11598, .F. ) ;
#11172 = ORIENTED_EDGE ( 'NONE', *, *, #3264, .T. ) ;
#11173 = CIRCLE ( 'NONE', #2660, 8.385254915620294014 ) ;
#11174 = ADVANCED_FACE ( 'NONE', ( #4867 ), #2553, .T. ) ;
#11175 = ORIENTED_EDGE ( 'NONE', *, *, #4980, .T. ) ;
#11176 = CARTESIAN_POINT ( 'NONE',  ( 1.738256873884670206, -152.7600787142097261, 0.2641564897029298753 ) ) ;
#11177 = ORIENTED_EDGE ( 'NONE', *, *, #10628, .F. ) ;
#11178 = AXIS2_PLACEMENT_3D ( 'NONE', #3370, #7652, #11929 ) ;
#11179 = CARTESIAN_POINT ( 'NONE',  ( 5.458723002619491282, -108.0793881314434088, -3.832583767769556005 ) ) ;
#11180 = EDGE_CURVE ( 'NONE', #8229, #6758, #7880, .T. ) ;
#11181 = DIRECTION ( 'NONE',  ( -2.797435172181481150E-17, 1.000000000000000000, -1.765856845898762549E-18 ) ) ;
#11182 = DIRECTION ( 'NONE',  ( 0.000000000000000000, 0.000000000000000000, 1.000000000000000000 ) ) ;
#11183 = ORIENTED_EDGE ( 'NONE', *, *, #11057, .F. ) ;
#11184 = ORIENTED_EDGE ( 'NONE', *, *, #9527, .T. ) ;
#11185 = DIRECTION ( 'NONE',  ( 0.000000000000000000, -0.000000000000000000, -1.000000000000000000 ) ) ;
#11186 = ORIENTED_EDGE ( 'NONE', *, *, #9175, .F. ) ;
#11187 = CARTESIAN_POINT ( 'NONE',  ( -1.786297911977085207, -149.6807761101056826, 0.8805805580279005840 ) ) ;
#11188 = VECTOR ( 'NONE', #10404, 1000.000000000000000 ) ;
#11189 = DIRECTION ( 'NONE',  ( -1.000000000000000000, 0.000000000000000000, 0.000000000000000000 ) ) ;
#11190 = PLANE ( 'NONE',  #13705 ) ;
#11191 = CARTESIAN_POINT ( 'NONE',  ( -40.73187278757662000, 100.6589795836331973, -1.037129925556720123 ) ) ;
#11192 = CARTESIAN_POINT ( 'NONE',  ( 25.00000000000000355, 120.0000000000000142, -2.499999999999998668 ) ) ;
#11193 = DIRECTION ( 'NONE',  ( -0.000000000000000000, -0.000000000000000000, -1.000000000000000000 ) ) ;
#11194 = CARTESIAN_POINT ( 'NONE',  ( 10.69381717166375445, 16.13466892210585613, 2.619229793989003951E-15 ) ) ;
#11195 = ORIENTED_EDGE ( 'NONE', *, *, #9718, .F. ) ;
#11196 = CARTESIAN_POINT ( 'NONE',  ( 4.318061424038318385, 91.66495677434029687, 2.521242278247964208 ) ) ;
#11197 = VERTEX_POINT ( 'NONE', #4729 ) ;
#11198 = CARTESIAN_POINT ( 'NONE',  ( 0.2321914886046761162, -147.1038961038780997, -14.56966866480831335 ) ) ;
#11199 = AXIS2_PLACEMENT_3D ( 'NONE', #6546, #6675, #4572 ) ;
#11200 = ORIENTED_EDGE ( 'NONE', *, *, #8076, .T. ) ;
#11201 = DIRECTION ( 'NONE',  ( 1.000000000000000000, 0.000000000000000000, 0.000000000000000000 ) ) ;
#11202 = DIRECTION ( 'NONE',  ( 0.000000000000000000, 0.000000000000000000, -1.000000000000000000 ) ) ;
#11203 = CARTESIAN_POINT ( 'NONE',  ( -54.35437857574594744, -62.63636364547547686, -19.28415345477669973 ) ) ;
#11204 = CIRCLE ( 'NONE', #8723, 24.99999999999998934 ) ;
#11205 = TOROIDAL_SURFACE ( 'NONE', #7837, 16.99999999999998934, 2.000000000000000000 ) ;
#11206 = DIRECTION ( 'NONE',  ( -0.000000000000000000, 0.000000000000000000, 1.000000000000000000 ) ) ;
#11207 = CARTESIAN_POINT ( 'NONE',  ( 15.29705854078140170, -19.91286587805129926, 3.746698755667524778E-15 ) ) ;
#11208 = CIRCLE ( 'NONE', #4464, 2.000000000000000000 ) ;
#11209 = CARTESIAN_POINT ( 'NONE',  ( -12.99553232110414136, -36.04913500549519512, -1.464178482349251183E-15 ) ) ;
#11210 = AXIS2_PLACEMENT_3D ( 'NONE', #1163, #10948, #3450 ) ;
#11211 = DIRECTION ( 'NONE',  ( 0.000000000000000000, 0.000000000000000000, 1.000000000000000000 ) ) ;
#11212 = ORIENTED_EDGE ( 'NONE', *, *, #3854, .F. ) ;
#11213 = ORIENTED_EDGE ( 'NONE', *, *, #1564, .T. ) ;
#11214 = CIRCLE ( 'NONE', #1347, 5.000000000000004441 ) ;
#11215 = CIRCLE ( 'NONE', #12344, 24.99999999999998934 ) ;
#11216 = VECTOR ( 'NONE', #9914, 1000.000000000000000 ) ;
#11217 = FACE_OUTER_BOUND ( 'NONE', #6499, .T. ) ;
#11218 = ORIENTED_EDGE ( 'NONE', *, *, #1279, .T. ) ;
#11219 = CARTESIAN_POINT ( 'NONE',  ( -12.99553232110413425, -36.04913500549519512, -25.99106464220827917 ) ) ;
#11220 = CARTESIAN_POINT ( 'NONE',  ( -8.385254915620299343, 78.67828027274755698, -1.304766718931246017E-15 ) ) ;
#11221 = LINE ( 'NONE', #13507, #18 ) ;
#11222 = CYLINDRICAL_SURFACE ( 'NONE', #9102, 15.29705854078139105 ) ;
#11223 = CARTESIAN_POINT ( 'NONE',  ( 8.591959856086345937, -92.28134618798193856, -0.7058139155579893353 ) ) ;
#11224 = VECTOR ( 'NONE', #9230, 1000.000000000000000 ) ;
#11225 = CARTESIAN_POINT ( 'NONE',  ( 8.385254915620294014, 50.40394642271930792, 9.813990265092209853E-16 ) ) ;
#11226 = VERTEX_POINT ( 'NONE', #9009 ) ;
#11227 = CIRCLE ( 'NONE', #12115, 79.99999999999997158 ) ;
#11228 = AXIS2_PLACEMENT_3D ( 'NONE', #11375, #9004, #13391 ) ;
#11229 = ORIENTED_EDGE ( 'NONE', *, *, #10382, .T. ) ;
#11230 = ORIENTED_EDGE ( 'NONE', *, *, #3163, .T. ) ;
#11231 = ORIENTED_EDGE ( 'NONE', *, *, #9635, .F. ) ;
#11232 = CARTESIAN_POINT ( 'NONE',  ( -2.504065471750553911E-13, 90.00000000000000000, 4.500000000000000888 ) ) ;
#11233 = DIRECTION ( 'NONE',  ( -2.797435172181481150E-17, 1.000000000000000000, -1.765856845898762549E-18 ) ) ;
#11234 = VERTEX_POINT ( 'NONE', #9079 ) ;
#11235 = DIRECTION ( 'NONE',  ( 1.000000000000000000, 0.000000000000000000, 0.000000000000000000 ) ) ;
#11236 =( LENGTH_UNIT ( ) NAMED_UNIT ( * ) SI_UNIT ( .MILLI., .METRE. ) );
#11237 = CIRCLE ( 'NONE', #5626, 66.24999999999978684 ) ;
#11238 = ADVANCED_FACE ( 'NONE', ( #11255 ), #12383, .T. ) ;
#11239 = DIRECTION ( 'NONE',  ( -0.9063077870366490485, -0.4226182617407014952, 0.000000000000000000 ) ) ;
#11240 = DIRECTION ( 'NONE',  ( -1.000000000000000000, 0.000000000000000000, 0.000000000000000000 ) ) ;
#11241 = CARTESIAN_POINT ( 'NONE',  ( 5.245880486154336886, -97.41991341991632680, 6.871249260556994365 ) ) ;
#11242 = CARTESIAN_POINT ( 'NONE',  ( -15.29705854078138749, -36.87585420866476227, 6.511747960273540061E-17 ) ) ;
#11243 = CARTESIAN_POINT ( 'NONE',  ( 25.00000000000000355, 120.0000000000000284, 2.500000000000000000 ) ) ;
#11244 = EDGE_CURVE ( 'NONE', #13844, #214, #3705, .T. ) ;
#11245 = DIRECTION ( 'NONE',  ( -2.797435172181481150E-17, 1.000000000000000000, -1.765856845898762549E-18 ) ) ;
#11246 = EDGE_CURVE ( 'NONE', #3535, #1501, #2589, .T. ) ;
#11247 = ORIENTED_EDGE ( 'NONE', *, *, #10784, .T. ) ;
#11248 = ORIENTED_EDGE ( 'NONE', *, *, #7140, .F. ) ;
#11249 = ORIENTED_EDGE ( 'NONE', *, *, #2082, .T. ) ;
#11250 = CARTESIAN_POINT ( 'NONE',  ( 0.6788169696763596273, -157.4020095821269649, 1.357710655470797834 ) ) ;
#11251 = VERTEX_POINT ( 'NONE', #2833 ) ;
#11252 = CARTESIAN_POINT ( 'NONE',  ( 5.164320697881710664, -107.4929201522786002, -4.328224869514438744 ) ) ;
#11253 = CARTESIAN_POINT ( 'NONE',  ( -25.00000000000000355, 120.0000000000000284, 2.500000000000000000 ) ) ;
#11254 = LINE ( 'NONE', #5925, #10760 ) ;
#11255 = FACE_OUTER_BOUND ( 'NONE', #2545, .T. ) ;
#11256 = FACE_OUTER_BOUND ( 'NONE', #4387, .T. ) ;
#11257 = VERTEX_POINT ( 'NONE', #4803 ) ;
#11258 = LINE ( 'NONE', #12593, #7065 ) ;
#11259 = CARTESIAN_POINT ( 'NONE',  ( 3.655937883597065952, -133.4173050103803746, -0.08043032631485191875 ) ) ;
#11260 = CARTESIAN_POINT ( 'NONE',  ( -35.00000000000000000, 25.00000000000000000, 7.500000000000000000 ) ) ;
#11261 = EDGE_CURVE ( 'NONE', #13136, #988, #6846, .T. ) ;
#11262 = DIRECTION ( 'NONE',  ( 1.000000000000000000, 0.000000000000000000, 0.000000000000000000 ) ) ;
#11263 = DIRECTION ( 'NONE',  ( -6.158143864569485777E-17, -2.736152283717910599E-16, 1.000000000000000000 ) ) ;
#11264 = CARTESIAN_POINT ( 'NONE',  ( -10.00000000000000711, 97.99999999999994316, -0.5000000000000000000 ) ) ;
#11265 = FACE_BOUND ( 'NONE', #4078, .T. ) ;
#11266 = EDGE_CURVE ( 'NONE', #3214, #5941, #7038, .T. ) ;
#11267 = EDGE_LOOP ( 'NONE', ( #10570, #1847, #9919, #4382 ) ) ;
#11268 = ORIENTED_EDGE ( 'NONE', *, *, #5573, .T. ) ;
#11269 = ORIENTED_EDGE ( 'NONE', *, *, #10136, .T. ) ;
#11270 = VERTEX_POINT ( 'NONE', #11317 ) ;
#11271 = CARTESIAN_POINT ( 'NONE',  ( 25.00000000000000355, 120.0000000000000142, 7.500000000000000000 ) ) ;
#11272 = CARTESIAN_POINT ( 'NONE',  ( 35.00000000000000000, -4.286263797015736496E-15, -4.000000000000000000 ) ) ;
#11273 = EDGE_CURVE ( 'NONE', #717, #8407, #9220, .T. ) ;
#11274 = CARTESIAN_POINT ( 'NONE',  ( 12.99579180576517068, 35.80917582696438473, -25.99158361153033070 ) ) ;
#11275 = B_SPLINE_CURVE_WITH_KNOTS ( 'NONE', 3,
 ( #11355, #1817, #12632, #3006 ),
 .UNSPECIFIED., .F., .F.,
 ( 4, 4 ),
 ( 0.000000000000000000, 1.000000000000000000 ),
 .UNSPECIFIED. ) ;
#11276 = DIRECTION ( 'NONE',  ( -6.158143864569485777E-17, -2.736152283717910599E-16, 1.000000000000000000 ) ) ;
#11277 = DIRECTION ( 'NONE',  ( -1.601283208593975514E-16, 1.000000000000000000, -0.000000000000000000 ) ) ;
#11278 = EDGE_CURVE ( 'NONE', #6854, #4529, #12238, .T. ) ;
#11279 = CARTESIAN_POINT ( 'NONE',  ( 12.99553232110414314, -36.04913500549519512, 3.182987412051232168E-15 ) ) ;
#11280 = CARTESIAN_POINT ( 'NONE',  ( 8.557187120185842488, -74.11437726413154792, 5.386762667206737021 ) ) ;
#11281 = ORIENTED_EDGE ( 'NONE', *, *, #7205, .F. ) ;
#11282 = AXIS2_PLACEMENT_3D ( 'NONE', #4070, #6250, #12646 ) ;
#11283 = VERTEX_POINT ( 'NONE', #7106 ) ;
#11284 = AXIS2_PLACEMENT_3D ( 'NONE', #8849, #1218, #13157 ) ;
#11285 = FACE_OUTER_BOUND ( 'NONE', #417, .T. ) ;
#11286 = ORIENTED_EDGE ( 'NONE', *, *, #3264, .F. ) ;
#11287 = CARTESIAN_POINT ( 'NONE',  ( 10.69346802281034137, 77.87317997377837742, 21.38693604562069694 ) ) ;
#11288 = CARTESIAN_POINT ( 'NONE',  ( -9.567184146940780565, -70.42919439405125104, -3.281027101740300989 ) ) ;
#11289 = FACE_OUTER_BOUND ( 'NONE', #9599, .T. ) ;
#11290 = CARTESIAN_POINT ( 'NONE',  ( 8.530666014548659248, -92.96565381893854862, 0.1002375751519047481 ) ) ;
#11291 = CARTESIAN_POINT ( 'NONE',  ( 8.385254915620292238, 15.32944684068712782, 1.008767855514154504E-15 ) ) ;
#11292 = ORIENTED_EDGE ( 'NONE', *, *, #6984, .T. ) ;
#11293 = ORIENTED_EDGE ( 'NONE', *, *, #1654, .F. ) ;
#11294 = ORIENTED_EDGE ( 'NONE', *, *, #3718, .T. ) ;
#11295 = EDGE_CURVE ( 'NONE', #8596, #13265, #11109, .T. ) ;
#11296 = ORIENTED_EDGE ( 'NONE', *, *, #2009, .F. ) ;
#11297 = LINE ( 'NONE', #4782, #10610 ) ;
#11298 = CARTESIAN_POINT ( 'NONE',  ( 3.385241169372599668, -79.21212121212093393, 9.605957155564981420 ) ) ;
#11299 = ORIENTED_EDGE ( 'NONE', *, *, #12213, .T. ) ;
#11300 = DIRECTION ( 'NONE',  ( -2.797435172181481150E-17, 1.000000000000000000, -1.765856845898762549E-18 ) ) ;
#11301 = CARTESIAN_POINT ( 'NONE',  ( 0.5797347049570226174, -122.9090909090902528, -5.796875383663783410 ) ) ;
#11302 = DIRECTION ( 'NONE',  ( 1.000000000000000000, 0.000000000000000000, 0.000000000000000000 ) ) ;
#11303 = DIRECTION ( 'NONE',  ( -1.000000000000000000, 0.000000000000000000, 0.000000000000000000 ) ) ;
#11304 =( NAMED_UNIT ( * ) PLANE_ANGLE_UNIT ( ) SI_UNIT ( $, .RADIAN. ) );
#11305 = AXIS2_PLACEMENT_3D ( 'NONE', #7057, #561, #13555 ) ;
#11306 = ORIENTED_EDGE ( 'NONE', *, *, #4228, .T. ) ;
#11307 = VERTEX_POINT ( 'NONE', #5779 ) ;
#11308 = VERTEX_POINT ( 'NONE', #465 ) ;
#11309 = DIRECTION ( 'NONE',  ( -0.000000000000000000, -0.000000000000000000, -1.000000000000000000 ) ) ;
#11310 = AXIS2_PLACEMENT_3D ( 'NONE', #2335, #1289, #5493 ) ;
#11311 = VERTEX_POINT ( 'NONE', #2626 ) ;
#11312 = EDGE_CURVE ( 'NONE', #12645, #4658, #10429, .T. ) ;
#11313 = CARTESIAN_POINT ( 'NONE',  ( -3.735183152658258177, -131.9664157448443973, 0.9167613680711519386 ) ) ;
#11314 = DIRECTION ( 'NONE',  ( -1.000000000000000000, 0.000000000000000000, 0.000000000000000000 ) ) ;
#11315 = EDGE_CURVE ( 'NONE', #8899, #13647, #4592, .T. ) ;
#11316 = DIRECTION ( 'NONE',  ( -6.158143864569485777E-17, -2.736152283717910599E-16, 1.000000000000000000 ) ) ;
#11317 = CARTESIAN_POINT ( 'NONE',  ( -4.547999443521272056, -70.00000000000000000, -2.077426547854386296 ) ) ;
#11318 = LINE ( 'NONE', #12443, #10316 ) ;
#11319 = ADVANCED_FACE ( 'NONE', ( #13229 ), #11016, .F. ) ;
#11320 = CIRCLE ( 'NONE', #9302, 9.000000000009000800 ) ;
#11321 = DIRECTION ( 'NONE',  ( 0.000000000000000000, 0.000000000000000000, 1.000000000000000000 ) ) ;
#11322 = CARTESIAN_POINT ( 'NONE',  ( 30.29366116764611760, 20.61262658154624816, -2.499999999999993783 ) ) ;
#11323 = CARTESIAN_POINT ( 'NONE',  ( 4.866961404864791341, 90.10495303670558087, -1.152376359967959507 ) ) ;
#11324 = DIRECTION ( 'NONE',  ( -1.000000000000000000, 0.000000000000000000, 0.000000000000000000 ) ) ;
#11325 = LINE ( 'NONE', #3823, #4642 ) ;
#11326 = DIRECTION ( 'NONE',  ( -1.000000000000000000, 0.000000000000000000, 0.000000000000000000 ) ) ;
#11327 = CARTESIAN_POINT ( 'NONE',  ( 8.385254915620285132, 62.45333659073424570, 16.77050983124058092 ) ) ;
#11328 = ADVANCED_FACE ( 'NONE', ( #2542 ), #2684, .T. ) ;
#11329 = ORIENTED_EDGE ( 'NONE', *, *, #10941, .T. ) ;
#11330 = EDGE_CURVE ( 'NONE', #12858, #3661, #11549, .T. ) ;
#11331 = CARTESIAN_POINT ( 'NONE',  ( 10.12341346682585552, -72.18181818173118813, 6.554034102529832317 ) ) ;
#11332 = CIRCLE ( 'NONE', #9994, 22.49999999999998934 ) ;
#11333 = ORIENTED_EDGE ( 'NONE', *, *, #9363, .T. ) ;
#11334 = EDGE_CURVE ( 'NONE', #6075, #1961, #3246, .T. ) ;
#11335 = ORIENTED_EDGE ( 'NONE', *, *, #139, .F. ) ;
#11336 = CARTESIAN_POINT ( 'NONE',  ( -4.942677383991351370, 90.01345119373434045, -0.7661926690451024147 ) ) ;
#11337 = EDGE_CURVE ( 'NONE', #3017, #9032, #8189, .T. ) ;
#11338 = CARTESIAN_POINT ( 'NONE',  ( -35.00000000000000000, -4.286263797015736496E-15, 7.500000000000000000 ) ) ;
#11339 = AXIS2_PLACEMENT_3D ( 'NONE', #1261, #5526, #8483 ) ;
#11340 = CARTESIAN_POINT ( 'NONE',  ( 3.794964386185876837, -129.7272727272737995, -2.624161884219710750 ) ) ;
#11341 = CARTESIAN_POINT ( 'NONE',  ( -10.69381717166375623, 6.709890972096426154, -1.333312310811123490E-15 ) ) ;
#11342 = CARTESIAN_POINT ( 'NONE',  ( -15.29705854078139637, 90.00000000000000000, -1.589271161308885878E-16 ) ) ;
#11343 = CARTESIAN_POINT ( 'NONE',  ( 10.69346802281034314, 21.32451227372186864, 2.619144277183852766E-15 ) ) ;
#11344 = CARTESIAN_POINT ( 'NONE',  ( 10.00000000000000000, 92.00000000000000000, -0.5000000000000000000 ) ) ;
#11345 = CIRCLE ( 'NONE', #3065, 22.99999999999999645 ) ;
#11346 = EDGE_LOOP ( 'NONE', ( #4549, #4765, #3917, #9962, #12977, #1043, #5127, #340, #2498, #10191, #13071, #2285 ) ) ;
#11347 = ADVANCED_FACE ( 'NONE', ( #8018 ), #10120, .T. ) ;
#11348 = FACE_OUTER_BOUND ( 'NONE', #4784, .T. ) ;
#11349 = EDGE_CURVE ( 'NONE', #11270, #9083, #7968, .T. ) ;
#11350 = ORIENTED_EDGE ( 'NONE', *, *, #2599, .F. ) ;
#11351 = ORIENTED_EDGE ( 'NONE', *, *, #2590, .F. ) ;
#11352 = CARTESIAN_POINT ( 'NONE',  ( -15.29705854078138749, -10.48808792804187284, -30.59411708156277854 ) ) ;
#11353 = CIRCLE ( 'NONE', #8663, 9.000000000009000800 ) ;
#11354 = CARTESIAN_POINT ( 'NONE',  ( -10.69346802281034847, -6.949821576306442594, -1.285027358575335329E-15 ) ) ;
#11355 = CARTESIAN_POINT ( 'NONE',  ( -8.385254915620294014, 59.82872437272870769, -1.056489625149731375E-16 ) ) ;
#11356 = CARTESIAN_POINT ( 'NONE',  ( -10.00000000000000000, 99.99999999999994316, -0.5000000000000000000 ) ) ;
#11357 = CARTESIAN_POINT ( 'NONE',  ( -5.081042958706433410, -118.5729905622867193, -1.793999374523247203 ) ) ;
#11358 = CARTESIAN_POINT ( 'NONE',  ( -8.385254915620294014, 59.82872437272870769, -1.238195484274846031E-15 ) ) ;
#11359 = VERTEX_POINT ( 'NONE', #7942 ) ;
#11360 = ORIENTED_EDGE ( 'NONE', *, *, #2672, .T. ) ;
#11361 = VERTEX_POINT ( 'NONE', #4791 ) ;
#11362 = ORIENTED_EDGE ( 'NONE', *, *, #792, .T. ) ;
#11363 = CARTESIAN_POINT ( 'NONE',  ( -8.385254915620292238, -12.94488700934118341, 2.285881734483108495E-17 ) ) ;
#11364 = CARTESIAN_POINT ( 'NONE',  ( 10.17548876272776859, -70.78787878787939292, 0.6371443735352817495 ) ) ;
#11365 = ORIENTED_EDGE ( 'NONE', *, *, #10784, .F. ) ;
#11366 = CARTESIAN_POINT ( 'NONE',  ( -35.45454545454546036, 140.4866414850956744, -2.500000000000000000 ) ) ;
#11367 = CARTESIAN_POINT ( 'NONE',  ( 10.69381717166374912, 44.40900277213413716, 21.38763434332751245 ) ) ;
#11368 = DIRECTION ( 'NONE',  ( -2.797435172181481150E-17, 1.000000000000000000, -1.765856845898762549E-18 ) ) ;
#11369 = DIRECTION ( 'NONE',  ( -2.797435172181481150E-17, 1.000000000000000000, -1.765856845898762549E-18 ) ) ;
#11370 = AXIS2_PLACEMENT_3D ( 'NONE', #7753, #9590, #1248 ) ;
#11371 = CARTESIAN_POINT ( 'NONE',  ( 0.1741500050819346779, -159.7355659919405184, -1.510064380825568708 ) ) ;
#11372 = DIRECTION ( 'NONE',  ( 1.000000000000000000, 1.850371707708595154E-15, 0.000000000000000000 ) ) ;
#11373 = ORIENTED_EDGE ( 'NONE', *, *, #892, .T. ) ;
#11374 = ORIENTED_EDGE ( 'NONE', *, *, #4890, .T. ) ;
#11375 = CARTESIAN_POINT ( 'NONE',  ( -35.20000000000000995, 106.4000000000000199, 0.5000000000000000000 ) ) ;
#11376 = VERTEX_POINT ( 'NONE', #389 ) ;
#11377 =( BOUNDED_SURFACE ( )  B_SPLINE_SURFACE ( 3, 3, ( 
 ( #11220, #8060, #8131, #13433 ),
 ( #6874, #3782, #11287, #9182 ),
 ( #13208, #13506, #13283, #1533 ),
 ( #4771, #7076, #7844, #12132 ) ),
 .UNSPECIFIED., .F., .F., .T. ) 
 B_SPLINE_SURFACE_WITH_KNOTS ( ( 4, 4 ),
 ( 4, 4 ),
 ( 0.000000000000000000, 1.000000000000000000 ),
 ( 0.000000000000000000, 1.000000000000000000 ),
 .UNSPECIFIED. ) 
 GEOMETRIC_REPRESENTATION_ITEM ( )  RATIONAL_B_SPLINE_SURFACE ( (
 ( 1.000000000000000000, 0.3333333333333334259, 0.3333333333333334259, 1.000000000000000000),
 ( 1.000000000000000000, 0.3333333333333334259, 0.3333333333333334259, 1.000000000000000000),
 ( 1.000000000000000000, 0.3333333333333334259, 0.3333333333333334259, 1.000000000000000000),
 ( 1.000000000000000000, 0.3333333333333334259, 0.3333333333333334259, 1.000000000000000000) ) ) 
 REPRESENTATION_ITEM ( '' )  SURFACE ( )  );
#11378 = CARTESIAN_POINT ( 'NONE',  ( 2.952295391231332111, -104.4213889740930199, -6.466433248859399185 ) ) ;
#11379 = AXIS2_PLACEMENT_3D ( 'NONE', #7496, #11840, #2367 ) ;
#11380 = DIRECTION ( 'NONE',  ( -6.158143864569485777E-17, -2.736152283717910599E-16, 1.000000000000000000 ) ) ;
#11381 = CARTESIAN_POINT ( 'NONE',  ( -25.00000000000000355, 120.0000000000000142, 2.499999999999999556 ) ) ;
#11382 = DIRECTION ( 'NONE',  ( -1.000000000000000000, 0.000000000000000000, 0.000000000000000000 ) ) ;
#11383 = DIRECTION ( 'NONE',  ( -6.158143864569485777E-17, -2.736152283717910599E-16, 1.000000000000000000 ) ) ;
#11384 = DIRECTION ( 'NONE',  ( 1.000000000000000000, 0.000000000000000000, -0.000000000000000000 ) ) ;
#11385 = CARTESIAN_POINT ( 'NONE',  ( -24.99999999999998934, -100.0000000000000000, 7.500000000000000000 ) ) ;
#11386 = CARTESIAN_POINT ( 'NONE',  ( 8.385254915620295790, 3.280056672672171381, -16.77050983124058448 ) ) ;
#11387 = EDGE_CURVE ( 'NONE', #8296, #11257, #6613, .T. ) ;
#11388 = CIRCLE ( 'NONE', #5546, 25.50000000002550138 ) ;
#11389 = DIRECTION ( 'NONE',  ( -0.000000000000000000, -1.000000000000000000, -0.000000000000000000 ) ) ;
#11390 = LINE ( 'NONE', #10002, #2996 ) ;
#11391 = AXIS2_PLACEMENT_3D ( 'NONE', #4991, #13584, #12224 ) ;
#11392 = PRODUCT_RELATED_PRODUCT_CATEGORY ( 'part', '', ( #10016 ) ) ;
#11393 = VERTEX_POINT ( 'NONE', #6955 ) ;
#11394 = CARTESIAN_POINT ( 'NONE',  ( 8.385254915620294014, 3.280056672672199358, 1.018788103988028997E-15 ) ) ;
#11395 = CARTESIAN_POINT ( 'NONE',  ( 17.09331748281897490, -62.63636361073249503, 11.08568378623573558 ) ) ;
#11396 = VERTEX_POINT ( 'NONE', #11242 ) ;
#11397 = CIRCLE ( 'NONE', #3544, 2.000000000000003109 ) ;
#11398 = ORIENTED_EDGE ( 'NONE', *, *, #12123, .T. ) ;
#11399 = CARTESIAN_POINT ( 'NONE',  ( 0.000000000000000000, -20.00000000000000000, 0.000000000000000000 ) ) ;
#11400 = CARTESIAN_POINT ( 'NONE',  ( 8.385254915620294014, 90.00000000000000000, 8.679704431140118580E-16 ) ) ;
#11401 = B_SPLINE_CURVE_WITH_KNOTS ( 'NONE', 3,
 ( #5889, #3768, #3545, #4893, #3624, #1383, #9942, #12339, #8051, #12192, #5662, #2726, #11280, #1674, #4610, #12040, #7833, #12119, #502, #2511, #6786, #11059, #10228, #1452 ),
 .UNSPECIFIED., .F., .F.,
 ( 4, 2, 2, 2, 2, 2, 2, 2, 2, 2, 2, 4 ),
 ( 0.000000000000000000, 0.002159622240606462202, 0.003239433360909706097, 0.004319244481212950425, 0.006478866721819439949, 0.008638488962425930340, 0.01079811120303241813, 0.01295773344363890592, 0.01403754456394215068, 0.01511735568424539371, 0.01619716680454863847, 0.01727697792485188150 ),
 .UNSPECIFIED. ) ;
#11402 =( BOUNDED_SURFACE ( )  B_SPLINE_SURFACE ( 3, 3, ( 
 ( #7649, #383, #6596, #11010 ),
 ( #3496, #4636, #6538, #6739 ),
 ( #1410, #2252, #8919, #1209 ),
 ( #8770, #10863, #5688, #3572 ) ),
 .UNSPECIFIED., .F., .F., .T. ) 
 B_SPLINE_SURFACE_WITH_KNOTS ( ( 4, 4 ),
 ( 4, 4 ),
 ( 0.000000000000000000, 1.000000000000000000 ),
 ( 0.000000000000000000, 1.000000000000000000 ),
 .UNSPECIFIED. ) 
 GEOMETRIC_REPRESENTATION_ITEM ( )  RATIONAL_B_SPLINE_SURFACE ( (
 ( 1.000000000000000000, 0.3333333333333334259, 0.3333333333333334259, 1.000000000000000000),
 ( 1.000000000000000000, 0.3333333333333334259, 0.3333333333333334259, 1.000000000000000000),
 ( 1.000000000000000000, 0.3333333333333334259, 0.3333333333333334259, 1.000000000000000000),
 ( 1.000000000000000000, 0.3333333333333334259, 0.3333333333333334259, 1.000000000000000000) ) ) 
 REPRESENTATION_ITEM ( '' )  SURFACE ( )  );
#11403 = CARTESIAN_POINT ( 'NONE',  ( -12.97432671026129292, -68.90909090921795155, -1.142286363974290175 ) ) ;
#11404 = EDGE_CURVE ( 'NONE', #1745, #8317, #5694, .T. ) ;
#11405 = DIRECTION ( 'NONE',  ( 0.000000000000000000, 0.000000000000000000, 1.000000000000000000 ) ) ;
#11406 = DIRECTION ( 'NONE',  ( -2.797435172181481150E-17, 1.000000000000000000, -1.765856845898762549E-18 ) ) ;
#11407 = ADVANCED_FACE ( 'NONE', ( #5621 ), #12904, .F. ) ;
#11408 = CARTESIAN_POINT ( 'NONE',  ( 12.99579180576517601, -30.16426982310158067, 0.000000000000000000 ) ) ;
#11409 = AXIS2_PLACEMENT_3D ( 'NONE', #12931, #4486, #9621 ) ;
#11410 = CARTESIAN_POINT ( 'NONE',  ( -4.390129302555909163, 91.34360472797649777, 2.393760519723236779 ) ) ;
#11411 = ADVANCED_FACE ( 'NONE', ( #9067 ), #3800, .T. ) ;
#11412 = ADVANCED_BREP_SHAPE_REPRESENTATION ( '', ( #3056, #8193 ), #12229 ) ;
#11413 = ADVANCED_FACE ( 'NONE', ( #8088 ), #2754, .T. ) ;
#11414 = CIRCLE ( 'NONE', #12770, 5.000000000000004441 ) ;
#11415 = VERTEX_POINT ( 'NONE', #13385 ) ;
#11416 = DIRECTION ( 'NONE',  ( -1.000000000000000000, -5.337610695313252124E-17, 0.000000000000000000 ) ) ;
#11417 = CIRCLE ( 'NONE', #224, 27.49999999999999289 ) ;
#11418 = VERTEX_POINT ( 'NONE', #4565 ) ;
#11419 = CARTESIAN_POINT ( 'NONE',  ( 10.69381717166375978, -12.13966492792242846, -21.38763434332751245 ) ) ;
#11420 = AXIS2_PLACEMENT_3D ( 'NONE', #2499, #1441, #4298 ) ;
#11421 = VECTOR ( 'NONE', #378, 1000.000000000000000 ) ;
#11422 = CARTESIAN_POINT ( 'NONE',  ( 34.26155123102906686, 108.1859746833188041, 0.7471162051235300527 ) ) ;
#11423 = DIRECTION ( 'NONE',  ( 0.000000000000000000, 0.000000000000000000, 1.000000000000000000 ) ) ;
#11424 = CARTESIAN_POINT ( 'NONE',  ( -2.517691654963332357E-15, 90.00000000000000000, -1.589271161308885878E-16 ) ) ;
#11425 = CARTESIAN_POINT ( 'NONE',  ( 5.863164109270496915, -98.21466495864295609, 5.258484191817180076 ) ) ;
#11426 = CARTESIAN_POINT ( 'NONE',  ( -12.99553232110414314, 48.77386654458962312, -3.284728769657734804E-15 ) ) ;
#11427 = ORIENTED_EDGE ( 'NONE', *, *, #4312, .T. ) ;
#11428 = ADVANCED_FACE ( 'NONE', ( #3579 ), #3734, .T. ) ;
#11429 = AXIS2_PLACEMENT_3D ( 'NONE', #4973, #6105, #10372 ) ;
#11430 = VERTEX_POINT ( 'NONE', #3504 ) ;
#11431 = ORIENTED_EDGE ( 'NONE', *, *, #3852, .F. ) ;
#11432 = DIRECTION ( 'NONE',  ( 0.9960067511297463483, -0.08927794634716618161, 4.818676322152979407E-17 ) ) ;
#11433 = CIRCLE ( 'NONE', #4482, 15.29705854078139105 ) ;
#11434 = AXIS2_PLACEMENT_3D ( 'NONE', #3669, #5928, #542 ) ;
#11435 = EDGE_LOOP ( 'NONE', ( #4953, #4064, #7487, #2847 ) ) ;
#11436 = CARTESIAN_POINT ( 'NONE',  ( -4.131580040049980695, 90.90692022676346085, -2.817507346490921716 ) ) ;
#11437 = ORIENTED_EDGE ( 'NONE', *, *, #9830, .F. ) ;
#11438 = FACE_OUTER_BOUND ( 'NONE', #5824, .T. ) ;
#11439 = VERTEX_POINT ( 'NONE', #13154 ) ;
#11440 = DIRECTION ( 'NONE',  ( -0.000000000000000000, -0.000000000000000000, -1.000000000000000000 ) ) ;
#11441 = B_SPLINE_CURVE_WITH_KNOTS ( 'NONE', 3,
 ( #8760, #4479, #20, #4405 ),
 .UNSPECIFIED., .F., .F.,
 ( 4, 4 ),
 ( 0.000000000000000000, 1.000000000000000000 ),
 .UNSPECIFIED. ) ;
#11442 = CIRCLE ( 'NONE', #12792, 2.000000000000000000 ) ;
#11443 = CARTESIAN_POINT ( 'NONE',  ( 8.385254915620290461, 43.60378069071538221, 2.053795118489799215E-15 ) ) ;
#11444 = AXIS2_PLACEMENT_3D ( 'NONE', #13125, #3480, #5384 ) ;
#11445 = FACE_OUTER_BOUND ( 'NONE', #1462, .T. ) ;
#11446 = AXIS2_PLACEMENT_3D ( 'NONE', #9422, #13735, #648 ) ;
#11447 = CARTESIAN_POINT ( 'NONE',  ( -2.625033373859935182, -142.3538918234897608, -0.5598298894019758665 ) ) ;
#11448 = DIRECTION ( 'NONE',  ( -6.158143864569485777E-17, -2.736152283717910599E-16, 1.000000000000000000 ) ) ;
#11449 = VERTEX_POINT ( 'NONE', #4074 ) ;
#11450 = ADVANCED_FACE ( 'NONE', ( #11445 ), #13728, .T. ) ;
#11451 = ORIENTED_EDGE ( 'NONE', *, *, #1370, .F. ) ;
#11452 = VERTEX_POINT ( 'NONE', #928 ) ;
#11453 = EDGE_LOOP ( 'NONE', ( #767, #9604, #13446, #3771, #13781, #2518, #7141, #7568 ) ) ;
#11454 = AXIS2_PLACEMENT_3D ( 'NONE', #11794, #5078, #13872 ) ;
#11455 = AXIS2_PLACEMENT_3D ( 'NONE', #5416, #7878, #13012 ) ;
#11456 = DIRECTION ( 'NONE',  ( 0.000000000000000000, 0.000000000000000000, 1.000000000000000000 ) ) ;
#11457 = CARTESIAN_POINT ( 'NONE',  ( -4.330127018922195425, 92.00000000000000000, 2.500000000000000000 ) ) ;
#11458 = CARTESIAN_POINT ( 'NONE',  ( -1.344244725514634808, -147.1541672456599485, 1.755023797081159298 ) ) ;
#11459 = CARTESIAN_POINT ( 'NONE',  ( -1.713057075430773901, -163.8787878553926589, -2.641018403485157595 ) ) ;
#11460 = CARTESIAN_POINT ( 'NONE',  ( -8.385254915620295790, 40.97916847270985130, -7.236334518677345233E-17 ) ) ;
#11461 = CARTESIAN_POINT ( 'NONE',  ( -35.00000000000000000, -4.286263797015736496E-15, 4.000000000000000000 ) ) ;
#11462 = DIRECTION ( 'NONE',  ( -1.000000000000000000, 0.000000000000000000, 0.000000000000000000 ) ) ;
#11463 = CARTESIAN_POINT ( 'NONE',  ( -10.00000000000000000, 90.00000000000000000, -0.5000000000000000000 ) ) ;
#11464 = CARTESIAN_POINT ( 'NONE',  ( 12.99553232110414136, 29.92431064457076673, 3.182987412051232168E-15 ) ) ;
#11465 = VECTOR ( 'NONE', #345, 1000.000000000000000 ) ;
#11466 = DIRECTION ( 'NONE',  ( -2.797435172181481150E-17, 1.000000000000000000, -1.765856845898762549E-18 ) ) ;
#11467 = ORIENTED_EDGE ( 'NONE', *, *, #10547, .F. ) ;
#11468 = EDGE_LOOP ( 'NONE', ( #3612, #734, #110, #7760 ) ) ;
#11469 = CARTESIAN_POINT ( 'NONE',  ( 2.247751904495991049, -65.63636362675833880, -0.1634371280250800362 ) ) ;
#11470 = VERTEX_POINT ( 'NONE', #3088 ) ;
#11471 = EDGE_CURVE ( 'NONE', #5663, #1107, #1698, .T. ) ;
#11472 = CARTESIAN_POINT ( 'NONE',  ( 8.385254915620292238, 22.12961257269105531, 9.855024866598291022E-16 ) ) ;
#11473 = ORIENTED_EDGE ( 'NONE', *, *, #7196, .F. ) ;
#11474 = CARTESIAN_POINT ( 'NONE',  ( 25.00000000000000355, 120.0000000000000142, 7.500000000000000000 ) ) ;
#11475 = CARTESIAN_POINT ( 'NONE',  ( -15.65588872828332612, -16.61546069029112260, 1.359866191199148089 ) ) ;
#11476 =( GEOMETRIC_REPRESENTATION_CONTEXT ( 3 ) GLOBAL_UNCERTAINTY_ASSIGNED_CONTEXT ( ( #4609 ) ) GLOBAL_UNIT_ASSIGNED_CONTEXT ( ( #4684, #12761, #10641 ) ) REPRESENTATION_CONTEXT ( 'NONE', 'WORKASPACE' ) );
#11477 = CARTESIAN_POINT ( 'NONE',  ( 15.66041902283167175, -22.75225252538438880, -1.300500990791221501 ) ) ;
#11478 = CARTESIAN_POINT ( 'NONE',  ( -2.940534136605371440, -72.18181818208977063, -3.082537950463050791 ) ) ;
#11479 = CARTESIAN_POINT ( 'NONE',  ( -39.99999999999999289, 120.0000000000000142, 0.5000000000000000000 ) ) ;
#11480 = CARTESIAN_POINT ( 'NONE',  ( 15.29705854078138927, 47.94714734142005597, 3.746698755667522411E-15 ) ) ;
#11481 = DIRECTION ( 'NONE',  ( -2.797435172181481150E-17, 1.000000000000000000, -1.765856845898762549E-18 ) ) ;
#11482 = CARTESIAN_POINT ( 'NONE',  ( -4.330127018922195425, 91.86461561432780343, 2.500000000000000000 ) ) ;
#11483 = VERTEX_POINT ( 'NONE', #13528 ) ;
#11484 = EDGE_CURVE ( 'NONE', #10464, #1545, #3039, .T. ) ;
#11485 = CARTESIAN_POINT ( 'NONE',  ( 25.00000000000000355, 120.0000000000000284, 0.5000000000000000000 ) ) ;
#11486 = ADVANCED_FACE ( 'NONE', ( #13656 ), #2821, .T. ) ;
#11487 =( BOUNDED_SURFACE ( )  B_SPLINE_SURFACE ( 3, 3, ( 
 ( #7887, #549, #3171, #10606 ),
 ( #9362, #10410, #6210, #11727 ),
 ( #8439, #6335, #8234, #13807 ),
 ( #13608, #7376, #11530, #5279 ) ),
 .UNSPECIFIED., .F., .F., .F. ) 
 B_SPLINE_SURFACE_WITH_KNOTS ( ( 4, 4 ),
 ( 4, 4 ),
 ( 0.000000000000000000, 1.000000000000000000 ),
 ( 0.000000000000000000, 1.000000000000000000 ),
 .UNSPECIFIED. ) 
 GEOMETRIC_REPRESENTATION_ITEM ( )  RATIONAL_B_SPLINE_SURFACE ( (
 ( 1.000000000000000000, 0.3333333333333334259, 0.3333333333333334259, 1.000000000000000000),
 ( 1.000000000000000000, 0.3333333333333334259, 0.3333333333333334259, 1.000000000000000000),
 ( 1.000000000000000000, 0.3333333333333334259, 0.3333333333333334259, 1.000000000000000000),
 ( 1.000000000000000000, 0.3333333333333334259, 0.3333333333333334259, 1.000000000000000000) ) ) 
 REPRESENTATION_ITEM ( '' )  SURFACE ( )  );
#11488 = AXIS2_PLACEMENT_3D ( 'NONE', #13045, #1382, #5661 ) ;
#11489 = EDGE_CURVE ( 'NONE', #10942, #1315, #8409, .T. ) ;
#11490 = CIRCLE ( 'NONE', #11918, 18.74900000001875000 ) ;
#11491 = CARTESIAN_POINT ( 'NONE',  ( 1.224646799147353217E-14, -100.0000000000000000, 0.000000000000000000 ) ) ;
#11492 = CARTESIAN_POINT ( 'NONE',  ( 35.65577094119244350, -20.24578327824959345, 2.499999999999994671 ) ) ;
#11493 = CARTESIAN_POINT ( 'NONE',  ( 32.50000000000000000, 4.286263797015736496E-15, 7.500000000000000000 ) ) ;
#11494 = LINE ( 'NONE', #10442, #9636 ) ;
#11495 = CIRCLE ( 'NONE', #11063, 40.00000000000001421 ) ;
#11496 = CARTESIAN_POINT ( 'NONE',  ( 2.034007080467508111, -145.4043805342818985, 1.227505828596866744 ) ) ;
#11497 = VECTOR ( 'NONE', #7295, 1000.000000000000000 ) ;
#11498 = CARTESIAN_POINT ( 'NONE',  ( 56.05919550416194141, -1.881564379087037553, -2.499999999999998224 ) ) ;
#11499 = VERTEX_POINT ( 'NONE', #7231 ) ;
#11500 = VERTEX_POINT ( 'NONE', #1700 ) ;
#11501 = ORIENTED_EDGE ( 'NONE', *, *, #9886, .T. ) ;
#11502 = EDGE_CURVE ( 'NONE', #8273, #6457, #6253, .T. ) ;
#11503 = EDGE_LOOP ( 'NONE', ( #4695, #536, #5634, #10529 ) ) ;
#11504 = DIRECTION ( 'NONE',  ( -1.000000000000000000, 0.000000000000000000, 0.000000000000000000 ) ) ;
#11505 = ORIENTED_EDGE ( 'NONE', *, *, #6515, .F. ) ;
#11506 = DIRECTION ( 'NONE',  ( -0.000000000000000000, -0.000000000000000000, -1.000000000000000000 ) ) ;
#11507 = ORIENTED_EDGE ( 'NONE', *, *, #3269, .T. ) ;
#11508 = ADVANCED_FACE ( 'NONE', ( #7299 ), #3868, .T. ) ;
#11509 = FACE_OUTER_BOUND ( 'NONE', #358, .T. ) ;
#11510 = AXIS2_PLACEMENT_3D ( 'NONE', #1926, #3964, #948 ) ;
#11511 = ADVANCED_FACE ( 'NONE', ( #8151, #8217 ), #10253, .F. ) ;
#11512 = CARTESIAN_POINT ( 'NONE',  ( -32.50000000000000000, -3.980102097228898626E-15, 7.500000000000000000 ) ) ;
#11513 = LINE ( 'NONE', #1969, #737 ) ;
#11514 = CARTESIAN_POINT ( 'NONE',  ( 25.00000000000000711, -34.99999999999999289, -7.500000000000000000 ) ) ;
#11515 = CARTESIAN_POINT ( 'NONE',  ( 34.99999999999958789, 1.091249486606660213E-13, 2.500000000000000000 ) ) ;
#11516 = CARTESIAN_POINT ( 'NONE',  ( 5.783304142548281845, -114.8445492426030938, -0.9050494705503316917 ) ) ;
#11517 = DIRECTION ( 'NONE',  ( -6.158143864569485777E-17, -2.736152283717910599E-16, 1.000000000000000000 ) ) ;
#11518 = ORIENTED_EDGE ( 'NONE', *, *, #7372, .F. ) ;
#11519 = VERTEX_POINT ( 'NONE', #5065 ) ;
#11520 = ORIENTED_EDGE ( 'NONE', *, *, #6079, .F. ) ;
#11521 = AXIS2_PLACEMENT_3D ( 'NONE', #12640, #10449, #7292 ) ;
#11522 = CARTESIAN_POINT ( 'NONE',  ( -2.531075078303758552, -137.7090071379864753, -1.916367648672105295 ) ) ;
#11523 = CARTESIAN_POINT ( 'NONE',  ( 33.39358510189357787, -25.44935030951552690, 2.499999999999992895 ) ) ;
#11524 = CARTESIAN_POINT ( 'NONE',  ( -8.385254915620295790, 40.97916847270985130, -2.162146219129312653E-15 ) ) ;
#11525 = CARTESIAN_POINT ( 'NONE',  ( 4.319514923984686838, -82.51052574872602463, -8.744483155999079216 ) ) ;
#11526 = EDGE_CURVE ( 'NONE', #3127, #11226, #8198, .T. ) ;
#11527 = CARTESIAN_POINT ( 'NONE',  ( 0.1425268984561593455, -158.0606060592834297, -0.6718241418694251843 ) ) ;
#11528 = CARTESIAN_POINT ( 'NONE',  ( 9.987599105592503079, -70.00000000000073896, 0.7388069301397282018 ) ) ;
#11529 = CIRCLE ( 'NONE', #13806, 22.99999999999999289 ) ;
#11530 = CARTESIAN_POINT ( 'NONE',  ( -15.29705854078138394, 19.67281349139177138, -30.59411708156277854 ) ) ;
#11531 = FACE_OUTER_BOUND ( 'NONE', #9331, .T. ) ;
#11532 = CARTESIAN_POINT ( 'NONE',  ( 25.00000000000000711, -99.22499053259345203, -1.700537903189176525 ) ) ;
#11533 = TOROIDAL_SURFACE ( 'NONE', #6173, 77.99999999999997158, 2.000000000000000000 ) ;
#11534 = DIRECTION ( 'NONE',  ( -1.000000000000000000, 0.000000000000000000, 0.000000000000000000 ) ) ;
#11535 = LINE ( 'NONE', #2978, #8120 ) ;
#11536 = ORIENTED_EDGE ( 'NONE', *, *, #8544, .F. ) ;
#11537 = DIRECTION ( 'NONE',  ( 0.000000000000000000, 0.000000000000000000, 1.000000000000000000 ) ) ;
#11538 = CARTESIAN_POINT ( 'NONE',  ( 25.00000000000000711, -34.99999999999999289, 7.500000000000000000 ) ) ;
#11539 = AXIS2_PLACEMENT_3D ( 'NONE', #49, #4303, #9445 ) ;
#11540 = ORIENTED_EDGE ( 'NONE', *, *, #3677, .T. ) ;
#11541 = CARTESIAN_POINT ( 'NONE',  ( 8.385254915620292238, 90.00000000000000000, 8.679704431140114636E-16 ) ) ;
#11542 = VERTEX_POINT ( 'NONE', #12504 ) ;
#11543 = DIRECTION ( 'NONE',  ( -0.000000000000000000, -0.000000000000000000, -1.000000000000000000 ) ) ;
#11544 = DIRECTION ( 'NONE',  ( 0.9960067511297464593, -0.08927794634716622324, 3.401418580343279473E-17 ) ) ;
#11545 = CARTESIAN_POINT ( 'NONE',  ( -39.00000000000000000, -3.673940397442060756E-15, 10.49999999999999822 ) ) ;
#11546 = CARTESIAN_POINT ( 'NONE',  ( -3.036220672062509340, -100.2727272727325953, -3.474096187147796222 ) ) ;
#11547 = PLANE ( 'NONE',  #4044 ) ;
#11548 = CARTESIAN_POINT ( 'NONE',  ( -8.385254915620297567, 50.40394642271930792, -1.204909866946646925E-15 ) ) ;
#11549 = CIRCLE ( 'NONE', #7284, 18.74900000001875355 ) ;
#11550 = CARTESIAN_POINT ( 'NONE',  ( 1.958204620527036102E-15, -69.99999999999998579, 1.236099792129133461E-16 ) ) ;
#11551 = FACE_OUTER_BOUND ( 'NONE', #13118, .T. ) ;
#11552 =( GEOMETRIC_REPRESENTATION_CONTEXT ( 3 ) GLOBAL_UNCERTAINTY_ASSIGNED_CONTEXT ( ( #4892 ) ) GLOBAL_UNIT_ASSIGNED_CONTEXT ( ( #2535, #6738, #4558 ) ) REPRESENTATION_CONTEXT ( 'NONE', 'WORKASPACE' ) );
#11553 = AXIS2_PLACEMENT_3D ( 'NONE', #3582, #2687, #12152 ) ;
#11554 = ORIENTED_EDGE ( 'NONE', *, *, #979, .T. ) ;
#11555 = CARTESIAN_POINT ( 'NONE',  ( -8.873256490562051013, -89.39237735558731401, 1.261745358756553470 ) ) ;
#11556 = AXIS2_PLACEMENT_3D ( 'NONE', #1906, #791, #4993 ) ;
#11557 = AXIS2_PLACEMENT_3D ( 'NONE', #6915, #1596, #1304 ) ;
#11558 = EDGE_LOOP ( 'NONE', ( #3415, #5153, #1305, #4882 ) ) ;
#11559 = CARTESIAN_POINT ( 'NONE',  ( -8.385254915620294014, -12.94488700934118341, -2.033253645871467057E-15 ) ) ;
#11560 = DIRECTION ( 'NONE',  ( -6.158143864569485777E-17, -2.736152283717910599E-16, 1.000000000000000000 ) ) ;
#11561 = CYLINDRICAL_SURFACE ( 'NONE', #201, 1.999999999999998224 ) ;
#11562 = DIRECTION ( 'NONE',  ( -6.158143864569485777E-17, -2.736152283717910599E-16, 1.000000000000000000 ) ) ;
#11563 = DIRECTION ( 'NONE',  ( 0.9960067511297463483, -0.08927794634716618161, 4.818676322152979407E-17 ) ) ;
#11564 = CARTESIAN_POINT ( 'NONE',  ( 1.377327726974544753, -148.4679005553610125, 1.573913393350005796 ) ) ;
#11565 = B_SPLINE_CURVE_WITH_KNOTS ( 'NONE', 3,
 ( #7741, #12027, #1101, #5429 ),
 .UNSPECIFIED., .F., .F.,
 ( 4, 4 ),
 ( 0.000000000000000000, 1.000000000000000000 ),
 .UNSPECIFIED. ) ;
#11566 = DIRECTION ( 'NONE',  ( 1.000000000000000000, 0.000000000000000000, 0.000000000000000000 ) ) ;
#11567 = ORIENTED_EDGE ( 'NONE', *, *, #11598, .T. ) ;
#11568 = VERTEX_POINT ( 'NONE', #10327 ) ;
#11569 = VERTEX_POINT ( 'NONE', #8425 ) ;
#11570 = DIRECTION ( 'NONE',  ( 2.797435172181644469E-17, -1.000000000000000000, 0.000000000000000000 ) ) ;
#11571 = CIRCLE ( 'NONE', #6641, 5.000000000000004441 ) ;
#11572 = VERTEX_POINT ( 'NONE', #9412 ) ;
#11573 = CARTESIAN_POINT ( 'NONE',  ( -12.97449437267217576, -39.59556244224027211, -3.094637852359278775E-15 ) ) ;
#11574 = ORIENTED_EDGE ( 'NONE', *, *, #8828, .T. ) ;
#11575 = CARTESIAN_POINT ( 'NONE',  ( 50.92330601230504783, -13.90964864522661415, -2.500000000000001776 ) ) ;
#11576 = APPLICATION_CONTEXT ( 'automotive_design' ) ;
#11577 = CARTESIAN_POINT ( 'NONE',  ( -10.00000000000000711, 139.9999999999999716, 2.500000000000000000 ) ) ;
#11578 = FACE_OUTER_BOUND ( 'NONE', #7872, .T. ) ;
#11579 = DIRECTION ( 'NONE',  ( -1.000000000000000000, 0.000000000000000000, 0.000000000000000000 ) ) ;
#11580 = CARTESIAN_POINT ( 'NONE',  ( 52.85884796071297131, 5.708463060827149604, -2.499999999999996447 ) ) ;
#11581 = EDGE_CURVE ( 'NONE', #5397, #9929, #13833, .T. ) ;
#11582 = CARTESIAN_POINT ( 'NONE',  ( 5.770584880507684922, -114.4337404266380531, -1.236082595024905695 ) ) ;
#11583 = EDGE_CURVE ( 'NONE', #11832, #11754, #10653, .T. ) ;
#11584 = DIRECTION ( 'NONE',  ( 0.5999999999999989786, -0.8000000000000008216, 0.000000000000000000 ) ) ;
#11585 = ADVANCED_FACE ( 'NONE', ( #9206 ), #12713, .T. ) ;
#11586 = ORIENTED_EDGE ( 'NONE', *, *, #632, .T. ) ;
#11587 = ORIENTED_EDGE ( 'NONE', *, *, #5225, .F. ) ;
#11588 = ORIENTED_EDGE ( 'NONE', *, *, #3189, .T. ) ;
#11589 = EDGE_CURVE ( 'NONE', #2825, #5181, #8630, .T. ) ;
#11590 = ADVANCED_FACE ( 'NONE', ( #3942 ), #2891, .F. ) ;
#11591 = CARTESIAN_POINT ( 'NONE',  ( 0.7069570379179631603, -145.1287559931344902, -2.290092706300334235 ) ) ;
#11592 = CARTESIAN_POINT ( 'NONE',  ( 12.99553232110412893, 39.34908859458022334, 25.99106464220826851 ) ) ;
#11593 = CARTESIAN_POINT ( 'NONE',  ( 10.69346802281034492, 40.17406817374066463, 1.263183422977906849E-15 ) ) ;
#11594 = CARTESIAN_POINT ( 'NONE',  ( 1.870037860061202206, -80.63037769710965108, -9.873254449573801494 ) ) ;
#11595 = CARTESIAN_POINT ( 'NONE',  ( 2.974540731479519701E-17, -1.063309978032472847, 1.877653204021102445E-18 ) ) ;
#11596 = CARTESIAN_POINT ( 'NONE',  ( 35.45454545454547457, 140.4866414850956460, -2.500000000000000000 ) ) ;
#11597 = CARTESIAN_POINT ( 'NONE',  ( -8.385254915620290461, 3.280056672672170492, -16.77050983124058803 ) ) ;
#11598 = EDGE_CURVE ( 'NONE', #6854, #6129, #12460, .T. ) ;
#11599 = CARTESIAN_POINT ( 'NONE',  ( -10.00000000000000000, 97.99999999999994316, -0.5000000000000000000 ) ) ;
#11600 = DIRECTION ( 'NONE',  ( -2.797435172181481150E-17, 1.000000000000000000, -1.765856845898762549E-18 ) ) ;
#11601 = LINE ( 'NONE', #10545, #8548 ) ;
#11602 = EDGE_CURVE ( 'NONE', #11415, #2835, #8874, .T. ) ;
#11603 = CARTESIAN_POINT ( 'NONE',  ( -30.72062512117230426, 25.13835616439067877, 0.000000000000000000 ) ) ;
#11604 = ORIENTED_EDGE ( 'NONE', *, *, #7624, .F. ) ;
#11605 = CARTESIAN_POINT ( 'NONE',  ( -15.29705854078139282, -10.48808792804187284, -1.836308454097519790E-15 ) ) ;
#11606 = EDGE_CURVE ( 'NONE', #8180, #3641, #11994, .T. ) ;
#11607 = ORIENTED_EDGE ( 'NONE', *, *, #1340, .T. ) ;
#11608 = FACE_OUTER_BOUND ( 'NONE', #12047, .T. ) ;
#11609 = DIRECTION ( 'NONE',  ( -1.000000000000000000, 0.000000000000000000, 0.000000000000000000 ) ) ;
#11610 = AXIS2_PLACEMENT_3D ( 'NONE', #11243, #10329, #5914 ) ;
#11611 = CARTESIAN_POINT ( 'NONE',  ( -12.65441377644764209, -89.44155844155457658, 5.520840484228807021 ) ) ;
#11612 = AXIS2_PLACEMENT_3D ( 'NONE', #6723, #3482, #10778 ) ;
#11613 = DIRECTION ( 'NONE',  ( 0.000000000000000000, 0.000000000000000000, -1.000000000000000000 ) ) ;
#11614 = B_SPLINE_CURVE_WITH_KNOTS ( 'NONE', 3,
 ( #4137, #7356, #5123, #2890 ),
 .UNSPECIFIED., .F., .F.,
 ( 4, 4 ),
 ( 0.000000000000000000, 1.000000000000000000 ),
 .UNSPECIFIED. ) ;
#11615 = CYLINDRICAL_SURFACE ( 'NONE', #7570, 2.000000000000000000 ) ;
#11616 = B_SPLINE_CURVE_WITH_KNOTS ( 'NONE', 3,
 ( #12485, #3005, #11623, #7337, #9464, #9252, #13639, #13567, #13772, #772, #10371, #7144, #2945, #8465, #7277, #11422, #10502, #7210 ),
 .UNSPECIFIED., .F., .F.,
 ( 4, 2, 2, 2, 2, 2, 2, 2, 4 ),
 ( 2.478944061730947031E-07, 0.0003651306916264191360, 0.0007300134888466652469, 0.001094896286066911412, 0.001459779083287157360, 0.001824661880507403309, 0.002189544677727649474, 0.002554427474947895422, 0.002919310272168141370 ),
 .UNSPECIFIED. ) ;
#11617 = VECTOR ( 'NONE', #12911, 1000.000000000000000 ) ;
#11618 = ORIENTED_EDGE ( 'NONE', *, *, #13073, .F. ) ;
#11619 = ORIENTED_EDGE ( 'NONE', *, *, #11244, .T. ) ;
#11620 = DIRECTION ( 'NONE',  ( -0.9960067511297463483, 0.08927794634716618161, -4.818676322152979407E-17 ) ) ;
#11621 = CARTESIAN_POINT ( 'NONE',  ( -21.99999999999999289, -97.00000000000000000, 7.500000000000000000 ) ) ;
#11622 = CIRCLE ( 'NONE', #8703, 9.000000000008999024 ) ;
#11623 = CARTESIAN_POINT ( 'NONE',  ( 34.92076574184287097, 106.7798134293914103, 2.447438947438307810 ) ) ;
#11624 = CARTESIAN_POINT ( 'NONE',  ( -10.69381717166375623, -2.714886977913000710, -2.620524279449481830E-15 ) ) ;
#11625 = DIRECTION ( 'NONE',  ( -0.000000000000000000, -0.000000000000000000, -1.000000000000000000 ) ) ;
#11626 = CARTESIAN_POINT ( 'NONE',  ( 25.00000000000000355, 120.0000000000000142, -7.500000000000000000 ) ) ;
#11627 = ORIENTED_EDGE ( 'NONE', *, *, #5924, .F. ) ;
#11628 = EDGE_LOOP ( 'NONE', ( #12282, #13504, #85, #8932 ) ) ;
#11629 = DIRECTION ( 'NONE',  ( -0.9923485843107423543, -2.797833471351478217E-17, -0.1234677578012386562 ) ) ;
#11630 = AXIS2_PLACEMENT_3D ( 'NONE', #8948, #13253, #12453 ) ;
#11631 = CARTESIAN_POINT ( 'NONE',  ( -15.29705854078139460, -8.601520358636511432, -1.842971270612889916E-15 ) ) ;
#11632 = ORIENTED_EDGE ( 'NONE', *, *, #6375, .T. ) ;
#11633 = EDGE_CURVE ( 'NONE', #4067, #8513, #10862, .T. ) ;
#11634 = CARTESIAN_POINT ( 'NONE',  ( -3.917571877187561391, 90.55481622686230025, -3.109379165354180241 ) ) ;
#11635 = AXIS2_PLACEMENT_3D ( 'NONE', #10351, #8446, #12733 ) ;
#11636 = EDGE_LOOP ( 'NONE', ( #9469, #2666, #10399, #2092, #11657, #6940, #2448, #7305 ) ) ;
#11637 = CARTESIAN_POINT ( 'NONE',  ( -8.385254915620294014, -24.99427717735608212, 4.413631546192547049E-17 ) ) ;
#11638 = ORIENTED_EDGE ( 'NONE', *, *, #2144, .F. ) ;
#11639 = LINE ( 'NONE', #2884, #10599 ) ;
#11640 = DIRECTION ( 'NONE',  ( 1.000000000000000000, 0.000000000000000000, -0.000000000000000000 ) ) ;
#11641 = CARTESIAN_POINT ( 'NONE',  ( -8.012933686896012375, -76.12121212232311507, -3.597289645623622967 ) ) ;
#11642 = CARTESIAN_POINT ( 'NONE',  ( 39.95750226049204912, 100.9609979968138731, -2.096206072712051949 ) ) ;
#11643 = CARTESIAN_POINT ( 'NONE',  ( -35.22727272727274794, 140.0412797136805523, -2.499999999999999556 ) ) ;
#11644 = AXIS2_PLACEMENT_3D ( 'NONE', #7998, #6931, #2662 ) ;
#11645 = CARTESIAN_POINT ( 'NONE',  ( 0.1431275062634679851, -159.4724345549973918, -1.503676168307738870 ) ) ;
#11646 = PLANE ( 'NONE',  #8850 ) ;
#11647 = ORIENTED_EDGE ( 'NONE', *, *, #719, .T. ) ;
#11648 = VECTOR ( 'NONE', #4351, 1000.000000000000000 ) ;
#11649 = CIRCLE ( 'NONE', #3566, 80.00000000000001421 ) ;
#11650 = EDGE_LOOP ( 'NONE', ( #7569, #12217, #5825, #7790 ) ) ;
#11651 = ORIENTED_EDGE ( 'NONE', *, *, #10243, .T. ) ;
#11652 = CARTESIAN_POINT ( 'NONE',  ( 0.3181136358666373787, -144.1302678916006812, -2.473221358873241016 ) ) ;
#11653 = DIRECTION ( 'NONE',  ( -1.000000000000000000, 0.000000000000000000, 0.000000000000000000 ) ) ;
#11654 = ADVANCED_FACE ( 'NONE', ( #12924 ), #219, .T. ) ;
#11655 = CYLINDRICAL_SURFACE ( 'NONE', #2670, 25.00000000000000711 ) ;
#11656 = ADVANCED_FACE ( 'NONE', ( #9548 ), #11779, .F. ) ;
#11657 = ORIENTED_EDGE ( 'NONE', *, *, #2870, .T. ) ;
#11658 = DIRECTION ( 'NONE',  ( -6.158143864569485777E-17, -2.736152283717910599E-16, 1.000000000000000000 ) ) ;
#11659 = CARTESIAN_POINT ( 'NONE',  ( -4.912780601956176163, -116.0400786845119114, -2.910660294657916314 ) ) ;
#11660 = CIRCLE ( 'NONE', #9428, 4.999999999999998224 ) ;
#11661 = CARTESIAN_POINT ( 'NONE',  ( -15.29705854078138927, 64.91013567203349055, -30.59411708156278564 ) ) ;
#11662 = CARTESIAN_POINT ( 'NONE',  ( 0.3001389404147826179, -80.00109702611953821, -10.02811144968829282 ) ) ;
#11663 = EDGE_CURVE ( 'NONE', #6588, #13109, #2063, .T. ) ;
#11664 = DIRECTION ( 'NONE',  ( -0.6466635011015190448, 0.7627754036039218200, -0.000000000000000000 ) ) ;
#11665 = EDGE_CURVE ( 'NONE', #4214, #7167, #4613, .T. ) ;
#11666 = LINE ( 'NONE', #2057, #4606 ) ;
#11667 = DIRECTION ( 'NONE',  ( -6.158143864569485777E-17, -2.736152283717910599E-16, 1.000000000000000000 ) ) ;
#11668 = CARTESIAN_POINT ( 'NONE',  ( 15.29705854078138927, 46.06057977201469100, 1.790347283588440388E-15 ) ) ;
#11669 = VECTOR ( 'NONE', #13088, 999.9999999999998863 ) ;
#11670 = AXIS2_PLACEMENT_3D ( 'NONE', #5175, #13176, #5785 ) ;
#11671 = CIRCLE ( 'NONE', #1599, 8.385254915620292238 ) ;
#11672 = CARTESIAN_POINT ( 'NONE',  ( 8.385254915620290461, -12.94488700934118341, 16.77050983124058803 ) ) ;
#11673 = EDGE_CURVE ( 'NONE', #6752, #5579, #1744, .T. ) ;
#11674 = ORIENTED_EDGE ( 'NONE', *, *, #289, .T. ) ;
#11675 = DIRECTION ( 'NONE',  ( 0.9960067511297464593, -0.08927794634716622324, 6.802837160686558945E-17 ) ) ;
#11676 = CARTESIAN_POINT ( 'NONE',  ( -3.913402758220056121, -81.93939393932039650, 9.205743832036068497 ) ) ;
#11677 = EDGE_CURVE ( 'NONE', #4883, #2829, #10263, .T. ) ;
#11678 = CARTESIAN_POINT ( 'NONE',  ( 12.85867081388377109, -161.0909090910740815, 2.071848600315243871 ) ) ;
#11679 = ADVANCED_FACE ( 'NONE', ( #13129 ), #9050, .F. ) ;
#11680 = VECTOR ( 'NONE', #6432, 1000.000000000000000 ) ;
#11681 = CARTESIAN_POINT ( 'NONE',  ( 10.00000000000000000, 97.99999999999994316, -2.500000000000000000 ) ) ;
#11682 = CARTESIAN_POINT ( 'NONE',  ( -10.69381717166375800, 25.55944687211528077, -2.674742811949561692E-15 ) ) ;
#11683 = CARTESIAN_POINT ( 'NONE',  ( -24.99999999999998934, -100.0000000000000000, 7.500000000000000000 ) ) ;
#11684 = LINE ( 'NONE', #4514, #2527 ) ;
#11685 = DIRECTION ( 'NONE',  ( -2.797435172181481150E-17, 1.000000000000000000, -1.765856845898762549E-18 ) ) ;
#11686 = ORIENTED_EDGE ( 'NONE', *, *, #1122, .T. ) ;
#11687 = ADVANCED_FACE ( 'NONE', ( #2444 ), #11222, .T. ) ;
#11688 = CARTESIAN_POINT ( 'NONE',  ( 0.000000000000000000, 0.000000000000000000, 0.000000000000000000 ) ) ;
#11689 = EDGE_LOOP ( 'NONE', ( #3359, #4506, #1910, #6794 ) ) ;
#11690 = CARTESIAN_POINT ( 'NONE',  ( 8.385254915620290461, 43.60378069071538221, -16.77050983124057737 ) ) ;
#11691 = CARTESIAN_POINT ( 'NONE',  ( 15.29705854078138572, 66.79670324143890525, 3.746698755667520834E-15 ) ) ;
#11692 = EDGE_CURVE ( 'NONE', #2348, #4358, #1040, .T. ) ;
#11693 = CARTESIAN_POINT ( 'NONE',  ( 10.69346802281034670, 30.74929022373126841, 1.274817642836897748E-15 ) ) ;
#11694 =( NAMED_UNIT ( * ) SI_UNIT ( $, .STERADIAN. ) SOLID_ANGLE_UNIT ( ) );
#11695 = CARTESIAN_POINT ( 'NONE',  ( 0.6082774961674913827, -152.6296145370220358, 1.642986734028079709 ) ) ;
#11696 = CARTESIAN_POINT ( 'NONE',  ( -29.00000000000000355, -5.021051876504148963E-15, -8.499999999999998224 ) ) ;
#11697 = ORIENTED_EDGE ( 'NONE', *, *, #9601, .F. ) ;
#11698 = ORIENTED_EDGE ( 'NONE', *, *, #6659, .T. ) ;
#11699 = ORIENTED_EDGE ( 'NONE', *, *, #12884, .F. ) ;
#11700 = CARTESIAN_POINT ( 'NONE',  ( -8.385254915620294014, 24.75422479069652582, -4.371241731156832241E-17 ) ) ;
#11701 = VECTOR ( 'NONE', #10903, 1000.000000000000000 ) ;
#11702 = CARTESIAN_POINT ( 'NONE',  ( -45.50000000000000711, 101.0000000000000000, -7.500000000000000000 ) ) ;
#11703 = CIRCLE ( 'NONE', #12398, 2.500000000000000444 ) ;
#11704 = CARTESIAN_POINT ( 'NONE',  ( 34.99999999999958789, 1.091249486606660213E-13, 2.500000000000000000 ) ) ;
#11705 = FACE_OUTER_BOUND ( 'NONE', #2381, .T. ) ;
#11706 = VERTEX_POINT ( 'NONE', #8000 ) ;
#11707 = CARTESIAN_POINT ( 'NONE',  ( 12.99579180576516535, 7.534841976936129448, 0.000000000000000000 ) ) ;
#11708 = DIRECTION ( 'NONE',  ( -2.797435172181481150E-17, 1.000000000000000000, -1.765856845898762549E-18 ) ) ;
#11709 = DIRECTION ( 'NONE',  ( -0.000000000000000000, -0.000000000000000000, -1.000000000000000000 ) ) ;
#11710 = CARTESIAN_POINT ( 'NONE',  ( 38.89115197531749857, 101.6687180808697377, -2.500000000000000000 ) ) ;
#11711 = CARTESIAN_POINT ( 'NONE',  ( 14.00979921278056040, -2.538005261501627086, -2.500000000000000888 ) ) ;
#11712 = AXIS2_PLACEMENT_3D ( 'NONE', #5459, #365, #8824 ) ;
#11713 = CARTESIAN_POINT ( 'NONE',  ( -0.01927387650405660430, -127.9334134464769335, 4.304559060634273848 ) ) ;
#11714 = DIRECTION ( 'NONE',  ( -1.000000000000000000, 0.000000000000000000, 0.000000000000000000 ) ) ;
#11715 = ORIENTED_EDGE ( 'NONE', *, *, #636, .T. ) ;
#11716 = ORIENTED_EDGE ( 'NONE', *, *, #3680, .F. ) ;
#11717 = DIRECTION ( 'NONE',  ( 0.000000000000000000, 0.000000000000000000, 1.000000000000000000 ) ) ;
#11718 = EDGE_LOOP ( 'NONE', ( #2352, #11876, #9212, #12466, #1617, #10200, #8669, #10829, #12435, #2451 ) ) ;
#11719 = AXIS2_PLACEMENT_3D ( 'NONE', #6273, #10940, #2188 ) ;
#11720 = CARTESIAN_POINT ( 'NONE',  ( 13.79311422413708499, -21.62638421600850691, -7.500000000000000000 ) ) ;
#11721 = VERTEX_POINT ( 'NONE', #13364 ) ;
#11722 = CARTESIAN_POINT ( 'NONE',  ( -25.00000000000000355, 120.0000000000000284, 2.500000000000000000 ) ) ;
#11723 = CARTESIAN_POINT ( 'NONE',  ( -5.570638609096381089, -114.5775772725542083, -1.854390173297266742 ) ) ;
#11724 = CARTESIAN_POINT ( 'NONE',  ( -8.385254915620292238, 5.904668890677671200, -2.066539263199666360E-15 ) ) ;
#11725 = CARTESIAN_POINT ( 'NONE',  ( -3.189539364161578128, -137.4545454545680627, 1.430838129453288143 ) ) ;
#11726 = CARTESIAN_POINT ( 'NONE',  ( 9.860966656300464095, -69.99999999999933209, 1.730751479080362865 ) ) ;
#11727 = CARTESIAN_POINT ( 'NONE',  ( -10.69346802281034492, 21.32451227372186864, -2.671336073255822280E-15 ) ) ;
#11728 = CARTESIAN_POINT ( 'NONE',  ( -10.13852281052241189, -69.87878787878712217, 0.9720347947262422128 ) ) ;
#11729 = CARTESIAN_POINT ( 'NONE',  ( 1.119237408740483668E-15, -40.00941361824963849, 7.065089693818137167E-17 ) ) ;
#11730 = CARTESIAN_POINT ( 'NONE',  ( 35.04450421339217314, 112.5597086678580609, 2.499999999999999556 ) ) ;
#11731 = TOROIDAL_SURFACE ( 'NONE', #7258, 42.00000000000001421, 2.000000000000000000 ) ;
#11732 = ADVANCED_FACE ( 'NONE', ( #2522 ), #3477, .T. ) ;
#11733 = EDGE_CURVE ( 'NONE', #4358, #2229, #5973, .T. ) ;
#11734 = ORIENTED_EDGE ( 'NONE', *, *, #8071, .T. ) ;
#11735 = CARTESIAN_POINT ( 'NONE',  ( 10.69381717166375267, 72.68333662216238622, 1.216686267861946676E-15 ) ) ;
#11736 = ORIENTED_EDGE ( 'NONE', *, *, #11180, .T. ) ;
#11737 = CARTESIAN_POINT ( 'NONE',  ( -57.42880470198044662, -62.63636363089489123, -5.311255545846308657 ) ) ;
#11738 = VERTEX_POINT ( 'NONE', #8823 ) ;
#11739 = AXIS2_PLACEMENT_3D ( 'NONE', #6434, #10697, #1109 ) ;
#11740 = DIRECTION ( 'NONE',  ( -2.797435172181481150E-17, 1.000000000000000000, -1.765856845898762549E-18 ) ) ;
#11741 = ORIENTED_EDGE ( 'NONE', *, *, #7546, .T. ) ;
#11742 = AXIS2_PLACEMENT_3D ( 'NONE', #184, #1292, #8866 ) ;
#11743 = FACE_OUTER_BOUND ( 'NONE', #1268, .T. ) ;
#11744 = FACE_OUTER_BOUND ( 'NONE', #9368, .T. ) ;
#11745 = CARTESIAN_POINT ( 'NONE',  ( 10.69346802281034314, 2.474956373702985601, 21.38693604562069694 ) ) ;
#11746 = AXIS2_PLACEMENT_3D ( 'NONE', #2130, #7393, #10485 ) ;
#11747 = CARTESIAN_POINT ( 'NONE',  ( 4.246087656260705501, -68.90909090936584391, -1.771789674505831247 ) ) ;
#11748 = CARTESIAN_POINT ( 'NONE',  ( -35.00000000000000711, -25.00000000000000711, 7.500000000000000000 ) ) ;
#11749 = CARTESIAN_POINT ( 'NONE',  ( 45.49999999999999289, 101.0000000000000142, 2.499999999999999556 ) ) ;
#11750 = CARTESIAN_POINT ( 'NONE',  ( 10.00000000000000000, 90.00000000000000000, -0.5000000000000000000 ) ) ;
#11751 = FACE_OUTER_BOUND ( 'NONE', #6186, .T. ) ;
#11752 = DIRECTION ( 'NONE',  ( 0.000000000000000000, 0.000000000000000000, 1.000000000000000000 ) ) ;
#11753 = AXIS2_PLACEMENT_3D ( 'NONE', #3248, #3449, #6756 ) ;
#11754 = VERTEX_POINT ( 'NONE', #5898 ) ;
#11755 = CIRCLE ( 'NONE', #799, 15.70031846811053455 ) ;
#11756 = EDGE_CURVE ( 'NONE', #30, #8596, #3712, .T. ) ;
#11757 = EDGE_CURVE ( 'NONE', #3278, #9863, #10916, .T. ) ;
#11758 =( NAMED_UNIT ( * ) PLANE_ANGLE_UNIT ( ) SI_UNIT ( $, .RADIAN. ) );
#11759 = ORIENTED_EDGE ( 'NONE', *, *, #10287, .F. ) ;
#11760 = CARTESIAN_POINT ( 'NONE',  ( 19.18070798040252711, 20.00000000000000000, 4.000000000000000000 ) ) ;
#11761 = DIRECTION ( 'NONE',  ( -0.8000000000000008216, 0.5999999999999988676, 0.000000000000000000 ) ) ;
#11762 = CARTESIAN_POINT ( 'NONE',  ( -10.69381717166375978, 53.83378072214353693, 21.38763434332750890 ) ) ;
#11763 = CIRCLE ( 'NONE', #3708, 9.000000000009002576 ) ;
#11764 = DIRECTION ( 'NONE',  ( 0.000000000000000000, 0.000000000000000000, 1.000000000000000000 ) ) ;
#11765 = CARTESIAN_POINT ( 'NONE',  ( -10.69346802281034847, 11.89973432371241202, 21.38693604562068629 ) ) ;
#11766 = ORIENTED_EDGE ( 'NONE', *, *, #11489, .F. ) ;
#11767 = VERTEX_POINT ( 'NONE', #9889 ) ;
#11768 = VERTEX_POINT ( 'NONE', #11151 ) ;
#11769 = AXIS2_PLACEMENT_3D ( 'NONE', #12986, #10715, #8616 ) ;
#11770 = ADVANCED_FACE ( 'NONE', ( #7766 ), #5744, .F. ) ;
#11771 = AXIS2_PLACEMENT_3D ( 'NONE', #3833, #7126, #2789 ) ;
#11772 = ORIENTED_EDGE ( 'NONE', *, *, #13704, .F. ) ;
#11773 = SPHERICAL_SURFACE ( 'NONE', #8969, 5.000000000000000000 ) ;
#11774 = ORIENTED_EDGE ( 'NONE', *, *, #11673, .F. ) ;
#11775 = EDGE_CURVE ( 'NONE', #9058, #7693, #4845, .T. ) ;
#11776 = DIRECTION ( 'NONE',  ( 5.551115123125776539E-17, -1.000000000000000000, -3.944304526105059027E-31 ) ) ;
#11777 = CARTESIAN_POINT ( 'NONE',  ( 40.00000000000000711, 100.0000000000000000, 0.5000000000000000000 ) ) ;
#11778 = AXIS2_PLACEMENT_3D ( 'NONE', #2491, #7672, #13104 ) ;
#11779 = PLANE ( 'NONE',  #6855 ) ;
#11780 = DIRECTION ( 'NONE',  ( -6.158143864569485777E-17, -2.736152283717910599E-16, 1.000000000000000000 ) ) ;
#11781 = CARTESIAN_POINT ( 'NONE',  ( -4.525117841679046293, -85.05660262901220392, 8.349665357795196030 ) ) ;
#11782 = CARTESIAN_POINT ( 'NONE',  ( -35.00000000000000000, -35.00000000000000000, -7.500000000000000000 ) ) ;
#11783 = ORIENTED_EDGE ( 'NONE', *, *, #4444, .F. ) ;
#11784 = ORIENTED_EDGE ( 'NONE', *, *, #7382, .T. ) ;
#11785 = VECTOR ( 'NONE', #11406, 1000.000000000000000 ) ;
#11786 = CARTESIAN_POINT ( 'NONE',  ( -4.330127018922197202, 91.82970358694005597, 2.500000000000001332 ) ) ;
#11787 = DIRECTION ( 'NONE',  ( -0.9960067511297463483, 0.08927794634716618161, -4.818676322152979407E-17 ) ) ;
#11788 = ORIENTED_EDGE ( 'NONE', *, *, #1639, .T. ) ;
#11789 = CARTESIAN_POINT ( 'NONE',  ( -10.69381717166375800, -2.714886977913000710, 21.38763434332750890 ) ) ;
#11790 = CARTESIAN_POINT ( 'NONE',  ( -8.385254915620292238, 40.97916847270985841, -16.77050983124058803 ) ) ;
#11791 = FACE_OUTER_BOUND ( 'NONE', #9439, .T. ) ;
#11792 = CARTESIAN_POINT ( 'NONE',  ( -10.69381717166375623, 6.709890972096426154, -2.632585121279762084E-15 ) ) ;
#11793 = CARTESIAN_POINT ( 'NONE',  ( 1.134746186788315070, -154.2164502155151524, 0.2399094883713628612 ) ) ;
#11794 = CARTESIAN_POINT ( 'NONE',  ( 34.99999999999958789, 1.091249486606660213E-13, 2.500000000000000000 ) ) ;
#11795 = DIRECTION ( 'NONE',  ( -1.000000000000000000, 0.000000000000000000, 0.000000000000000000 ) ) ;
#11796 = CARTESIAN_POINT ( 'NONE',  ( 32.72727272727274084, 135.1423002281141805, -2.500000000000000000 ) ) ;
#11797 = CARTESIAN_POINT ( 'NONE',  ( -9.940250983052290934, -69.87878787878452158, -1.425521750854495506 ) ) ;
#11798 = CARTESIAN_POINT ( 'NONE',  ( 12.99553232110413958, -17.19957910547634228, 25.99106464220828983 ) ) ;
#11799 = DIRECTION ( 'NONE',  ( -0.000000000000000000, -0.000000000000000000, -1.000000000000000000 ) ) ;
#11800 = DIRECTION ( 'NONE',  ( 1.000000000000000000, 0.000000000000000000, 0.000000000000000000 ) ) ;
#11801 = LINE ( 'NONE', #6478, #4235 ) ;
#11802 = EDGE_LOOP ( 'NONE', ( #13069, #3640, #9055, #3897 ) ) ;
#11803 = DIRECTION ( 'NONE',  ( -0.000000000000000000, 1.000000000000000000, -0.000000000000000000 ) ) ;
#11804 = ORIENTED_EDGE ( 'NONE', *, *, #6600, .F. ) ;
#11805 = CARTESIAN_POINT ( 'NONE',  ( -35.00000000000000000, -4.286263797015736496E-15, -10.49999999999999822 ) ) ;
#11806 = VERTEX_POINT ( 'NONE', #7926 ) ;
#11807 = CYLINDRICAL_SURFACE ( 'NONE', #3021, 9.000000000008999024 ) ;
#11808 = CARTESIAN_POINT ( 'NONE',  ( 34.99999999999958789, 1.063887963769481123E-13, 12.50000000000000000 ) ) ;
#11809 = EDGE_CURVE ( 'NONE', #3010, #769, #4378, .T. ) ;
#11810 = CARTESIAN_POINT ( 'NONE',  ( -8.385254915620297567, 24.75422479069652937, 16.77050983124058803 ) ) ;
#11811 = DIRECTION ( 'NONE',  ( 0.000000000000000000, 0.000000000000000000, 1.000000000000000000 ) ) ;
#11812 = CARTESIAN_POINT ( 'NONE',  ( -18.54049621773915746, -20.00000000000000000, 7.500000000000000000 ) ) ;
#11813 = CARTESIAN_POINT ( 'NONE',  ( -15.29705854078138749, 10.24803554138234496, -3.766461023514128305E-15 ) ) ;
#11814 = CARTESIAN_POINT ( 'NONE',  ( 40.50666510048448288, 100.7305537260640307, 1.531269357928750185 ) ) ;
#11815 = CARTESIAN_POINT ( 'NONE',  ( -28.15981099771517648, -27.70535714287384366, 4.000000000000000000 ) ) ;
#11816 = DIRECTION ( 'NONE',  ( 0.000000000000000000, 0.000000000000000000, 1.000000000000000000 ) ) ;
#11817 = ORIENTED_EDGE ( 'NONE', *, *, #5450, .F. ) ;
#11818 = AXIS2_PLACEMENT_3D ( 'NONE', #9397, #1887, #7341 ) ;
#11819 = AXIS2_PLACEMENT_3D ( 'NONE', #8481, #2100, #2442 ) ;
#11820 = EDGE_CURVE ( 'NONE', #11393, #8022, #3940, .T. ) ;
#11821 = SURFACE_SIDE_STYLE ('',( #1177 ) ) ;
#11822 = ORIENTED_EDGE ( 'NONE', *, *, #11006, .F. ) ;
#11823 = EDGE_CURVE ( 'NONE', #9570, #10854, #2887, .T. ) ;
#11824 = CARTESIAN_POINT ( 'NONE',  ( -35.00000000000000000, -4.286263797015736496E-15, -7.500000000000000000 ) ) ;
#11825 = ADVANCED_FACE ( 'NONE', ( #8063 ), #6107, .T. ) ;
#11826 = FACE_OUTER_BOUND ( 'NONE', #1542, .T. ) ;
#11827 = EDGE_CURVE ( 'NONE', #6325, #10679, #9318, .T. ) ;
#11828 = DIRECTION ( 'NONE',  ( -0.000000000000000000, -0.000000000000000000, -1.000000000000000000 ) ) ;
#11829 = VECTOR ( 'NONE', #13893, 1000.000000000000000 ) ;
#11830 = PLANE ( 'NONE',  #10273 ) ;
#11831 = AXIS2_PLACEMENT_3D ( 'NONE', #12580, #11708, #6316 ) ;
#11832 = VERTEX_POINT ( 'NONE', #1819 ) ;
#11833 = ORIENTED_EDGE ( 'NONE', *, *, #1741, .T. ) ;
#11834 = ORIENTED_EDGE ( 'NONE', *, *, #5390, .F. ) ;
#11835 = LINE ( 'NONE', #212, #12116 ) ;
#11836 = AXIS2_PLACEMENT_3D ( 'NONE', #5566, #2079, #8459 ) ;
#11837 = VERTEX_POINT ( 'NONE', #6425 ) ;
#11838 = DIRECTION ( 'NONE',  ( 0.000000000000000000, 0.000000000000000000, -1.000000000000000000 ) ) ;
#11839 = VECTOR ( 'NONE', #10425, 1000.000000000000000 ) ;
#11840 = DIRECTION ( 'NONE',  ( 0.000000000000000000, 0.000000000000000000, 1.000000000000000000 ) ) ;
#11841 =( BOUNDED_SURFACE ( )  B_SPLINE_SURFACE ( 3, 3, ( 
 ( #4829, #3765, #6856, #1797 ),
 ( #5804, #11274, #5883, #9103 ),
 ( #10156, #9165, #11134, #13490 ),
 ( #13556, #3975, #761, #8251 ) ),
 .UNSPECIFIED., .F., .F., .T. ) 
 B_SPLINE_SURFACE_WITH_KNOTS ( ( 4, 4 ),
 ( 4, 4 ),
 ( 0.000000000000000000, 1.000000000000000000 ),
 ( 0.000000000000000000, 1.000000000000000000 ),
 .UNSPECIFIED. ) 
 GEOMETRIC_REPRESENTATION_ITEM ( )  RATIONAL_B_SPLINE_SURFACE ( (
 ( 1.000000000000000000, 0.3333333333333334259, 0.3333333333333334259, 1.000000000000000000),
 ( 1.000000000000000000, 0.3333333333333334259, 0.3333333333333334259, 1.000000000000000000),
 ( 1.000000000000000000, 0.3333333333333334259, 0.3333333333333334259, 1.000000000000000000),
 ( 1.000000000000000000, 0.3333333333333334259, 0.3333333333333334259, 1.000000000000000000) ) ) 
 REPRESENTATION_ITEM ( '' )  SURFACE ( )  );
#11842 = CARTESIAN_POINT ( 'NONE',  ( -35.22727272727274794, 140.0412797136805523, 7.500000000000000000 ) ) ;
#11843 = EDGE_CURVE ( 'NONE', #1753, #9666, #7740, .T. ) ;
#11844 = CARTESIAN_POINT ( 'NONE',  ( 40.24692185806991063, 100.8304034607652113, -1.836112450589440614 ) ) ;
#11845 = DIRECTION ( 'NONE',  ( 0.000000000000000000, -0.000000000000000000, 1.000000000000000000 ) ) ;
#11846 = CARTESIAN_POINT ( 'NONE',  ( -1.409802153637102151, -82.49939887521887272, 9.633183655277679946 ) ) ;
#11847 = CARTESIAN_POINT ( 'NONE',  ( 35.00000000000009237, 91.25000000000046896, -7.500000000000000000 ) ) ;
#11848 = ORIENTED_EDGE ( 'NONE', *, *, #11387, .T. ) ;
#11849 = AXIS2_PLACEMENT_3D ( 'NONE', #10796, #1077, #9625 ) ;
#11850 = VERTEX_POINT ( 'NONE', #1100 ) ;
#11851 = ORIENTED_EDGE ( 'NONE', *, *, #1364, .T. ) ;
#11852 = AXIS2_PLACEMENT_3D ( 'NONE', #10416, #1997, #7118 ) ;
#11853 = CARTESIAN_POINT ( 'NONE',  ( -2.766098618134340104, 90.01525736159538837, 4.178197917109232051 ) ) ;
#11854 = CARTESIAN_POINT ( 'NONE',  ( -0.2462491701482444895, -80.00109949033800660, 10.02538131881691008 ) ) ;
#11855 = ORIENTED_EDGE ( 'NONE', *, *, #11273, .T. ) ;
#11856 = CARTESIAN_POINT ( 'NONE',  ( -15.29705854078138749, 10.24803554138234496, -1.809656371776380929E-17 ) ) ;
#11857 = CARTESIAN_POINT ( 'NONE',  ( 1.214223716166046518, -80.16973037252847689, -10.05352466437349612 ) ) ;
#11858 = CARTESIAN_POINT ( 'NONE',  ( 8.385254915620294014, 5.904668890677672088, -16.77050983124058092 ) ) ;
#11859 = AXIS2_PLACEMENT_3D ( 'NONE', #3751, #9151, #3676 ) ;
#11860 = CARTESIAN_POINT ( 'NONE',  ( 22.84091969677297485, -17.29701610032388359, 2.499999999999994227 ) ) ;
#11861 = CARTESIAN_POINT ( 'NONE',  ( 0.03865624730933259895, -158.0606060602139564, 1.868422726205244189 ) ) ;
#11862 = EDGE_CURVE ( 'NONE', #6545, #2529, #12237, .T. ) ;
#11863 = CIRCLE ( 'NONE', #8291, 2.500000000000002220 ) ;
#11864 = CARTESIAN_POINT ( 'NONE',  ( -9.997547090296809102, -68.99999999999981526, -0.6397344882394256915 ) ) ;
#11865 = CIRCLE ( 'NONE', #2453, 24.99999999999998934 ) ;
#11866 = DIRECTION ( 'NONE',  ( -1.000000000000000000, 0.000000000000000000, 0.000000000000000000 ) ) ;
#11867 = CARTESIAN_POINT ( 'NONE',  ( -32.50000000000000000, 110.0000000000000142, -2.499999999999999556 ) ) ;
#11868 = EDGE_LOOP ( 'NONE', ( #1514, #13439, #4079, #6774 ) ) ;
#11869 = DIRECTION ( 'NONE',  ( -1.224646799147353207E-16, 1.000000000000000000, -0.000000000000000000 ) ) ;
#11870 = CARTESIAN_POINT ( 'NONE',  ( -12.99579180576516535, 73.50828762700210461, -25.99158361153033425 ) ) ;
#11871 = COLOUR_RGB ( '', 0.31764706, 0.68627451, 0.89019608) ;
#11872 = ORIENTED_EDGE ( 'NONE', *, *, #4051, .T. ) ;
#11873 = AXIS2_PLACEMENT_3D ( 'NONE', #2136, #5097, #6423 ) ;
#11874 = CARTESIAN_POINT ( 'NONE',  ( 55.00383357371546822, 6.846651893462920135, -2.499999999999995559 ) ) ;
#11875 = CARTESIAN_POINT ( 'NONE',  ( 6.991987007918878033E-16, -24.99427717735608212, 4.413631546192547049E-17 ) ) ;
#11876 = ORIENTED_EDGE ( 'NONE', *, *, #13309, .T. ) ;
#11877 = CARTESIAN_POINT ( 'NONE',  ( -39.99999999999999289, 120.0000000000000284, 2.500000000000000000 ) ) ;
#11878 = ORIENTED_EDGE ( 'NONE', *, *, #3773, .F. ) ;
#11879 = CARTESIAN_POINT ( 'NONE',  ( 0.000000000000000000, 71.01020514433645303, -2.500000000000000000 ) ) ;
#11880 = CARTESIAN_POINT ( 'NONE',  ( -12.99553232110414491, 1.649976794542511893, -1.597320951662050367E-15 ) ) ;
#11881 = CARTESIAN_POINT ( 'NONE',  ( 34.40224804986664964, 107.7695571918731474, -1.740729949763267337 ) ) ;
#11882 = PRESENTATION_LAYER_ASSIGNMENT (  '', '', ( #1595 ) ) ;
#11883 = DIRECTION ( 'NONE',  ( -0.4545454545454548634, 0.8907235428302464619, 0.000000000000000000 ) ) ;
#11884 = DIRECTION ( 'NONE',  ( 1.000000000000000000, 0.000000000000000000, 0.000000000000000000 ) ) ;
#11885 = CARTESIAN_POINT ( 'NONE',  ( 39.10039359579067764, 101.4951258812516812, 2.486679384192855835 ) ) ;
#11886 = AXIS2_PLACEMENT_3D ( 'NONE', #9179, #2659, #5740 ) ;
#11887 = CARTESIAN_POINT ( 'NONE',  ( 50.48962708925064646, 14.39101985375337556, -2.499999999999993783 ) ) ;
#11888 = AXIS2_PLACEMENT_3D ( 'NONE', #3514, #12305, #8939 ) ;
#11889 = DIRECTION ( 'NONE',  ( -0.000000000000000000, -0.000000000000000000, -1.000000000000000000 ) ) ;
#11890 = EDGE_CURVE ( 'NONE', #3535, #1419, #6192, .T. ) ;
#11891 = CARTESIAN_POINT ( 'NONE',  ( 9.628507540654561270E-16, -34.41905512736551032, 6.077912412602530076E-17 ) ) ;
#11892 = EDGE_LOOP ( 'NONE', ( #1888, #10704, #4092, #11200 ) ) ;
#11893 = B_SPLINE_CURVE_WITH_KNOTS ( 'NONE', 3,
 ( #5876, #4591, #2637, #10147 ),
 .UNSPECIFIED., .F., .F.,
 ( 4, 4 ),
 ( 0.000000000000000000, 1.000000000000000000 ),
 .UNSPECIFIED. ) ;
#11894 = VERTEX_POINT ( 'NONE', #3122 ) ;
#11895 = EDGE_LOOP ( 'NONE', ( #9125, #2163, #9835, #7854, #12967, #4337, #5624, #12592, #265 ) ) ;
#11896 = DIRECTION ( 'NONE',  ( -1.000000000000000000, 0.000000000000000000, 0.000000000000000000 ) ) ;
#11897 = DIRECTION ( 'NONE',  ( 1.000000000000000000, 1.632680918566407779E-15, 0.000000000000000000 ) ) ;
#11898 = DIRECTION ( 'NONE',  ( -0.000000000000000000, -0.000000000000000000, -1.000000000000000000 ) ) ;
#11899 = DIRECTION ( 'NONE',  ( -6.158143864569485777E-17, -2.736152283717910599E-16, 1.000000000000000000 ) ) ;
#11900 = ORIENTED_EDGE ( 'NONE', *, *, #4625, .T. ) ;
#11901 = EDGE_CURVE ( 'NONE', #9044, #10464, #3850, .T. ) ;
#11902 = ORIENTED_EDGE ( 'NONE', *, *, #9530, .T. ) ;
#11903 = EDGE_CURVE ( 'NONE', #13483, #5724, #4848, .T. ) ;
#11904 = ORIENTED_EDGE ( 'NONE', *, *, #6112, .F. ) ;
#11905 = DIRECTION ( 'NONE',  ( -2.797435172181481150E-17, 1.000000000000000000, -1.765856845898762549E-18 ) ) ;
#11906 = ORIENTED_EDGE ( 'NONE', *, *, #796, .T. ) ;
#11907 = CARTESIAN_POINT ( 'NONE',  ( -60.00000000000001421, -4.286263797015736496E-15, 4.000000000000000000 ) ) ;
#11908 = DIRECTION ( 'NONE',  ( 0.9960067511297463483, -0.08927794634716618161, 4.818676322152979407E-17 ) ) ;
#11909 = DIRECTION ( 'NONE',  ( 0.000000000000000000, 0.000000000000000000, -1.000000000000000000 ) ) ;
#11910 = CARTESIAN_POINT ( 'NONE',  ( -34.33153323985096250, 107.9636705364999472, -1.438784920770796338 ) ) ;
#11911 = DIRECTION ( 'NONE',  ( -6.158143864569485777E-17, -2.736152283717910599E-16, 1.000000000000000000 ) ) ;
#11912 = CARTESIAN_POINT ( 'NONE',  ( -12.99579180576517246, 64.08350967699263379, -1.817850092276246042E-15 ) ) ;
#11913 = FACE_OUTER_BOUND ( 'NONE', #1373, .T. ) ;
#11914 = AXIS2_PLACEMENT_3D ( 'NONE', #12893, #11811, #1294 ) ;
#11915 = VERTEX_POINT ( 'NONE', #7078 ) ;
#11916 = ORIENTED_EDGE ( 'NONE', *, *, #1458, .T. ) ;
#11917 = VERTEX_POINT ( 'NONE', #11356 ) ;
#11918 = AXIS2_PLACEMENT_3D ( 'NONE', #8526, #189, #5564 ) ;
#11919 = EDGE_CURVE ( 'NONE', #5181, #11519, #1927, .T. ) ;
#11920 = EDGE_CURVE ( 'NONE', #11483, #13056, #774, .T. ) ;
#11921 = CARTESIAN_POINT ( 'NONE',  ( -3.159504973698680885, 90.09612598291141694, 3.878748273749980768 ) ) ;
#11922 = CARTESIAN_POINT ( 'NONE',  ( 0.1244050240884003455, -80.00111861713446615, 10.00661217103304068 ) ) ;
#11923 = ORIENTED_EDGE ( 'NONE', *, *, #3172, .F. ) ;
#11924 = DIRECTION ( 'NONE',  ( 1.000000000000000000, 0.000000000000000000, 0.000000000000000000 ) ) ;
#11925 = PRESENTATION_STYLE_ASSIGNMENT (( #7648 ) ) ;
#11926 = CARTESIAN_POINT ( 'NONE',  ( 15.29705854078139105, 36.63580182200523438, 3.746698755667522411E-15 ) ) ;
#11927 = DIRECTION ( 'NONE',  ( -0.000000000000000000, -0.000000000000000000, -1.000000000000000000 ) ) ;
#11928 = CIRCLE ( 'NONE', #3411, 1.999999999999998224 ) ;
#11929 = DIRECTION ( 'NONE',  ( 0.9960067511297463483, -0.08927794634716620936, 4.626175998653454121E-17 ) ) ;
#11930 = FACE_OUTER_BOUND ( 'NONE', #5670, .T. ) ;
#11931 = CARTESIAN_POINT ( 'NONE',  ( 12.99579180576516535, 45.23395377697384134, 0.000000000000000000 ) ) ;
#11932 = CARTESIAN_POINT ( 'NONE',  ( -10.69346802281034847, -16.37459952631584059, 21.38693604562068984 ) ) ;
#11933 = DIRECTION ( 'NONE',  ( 6.158143864569485777E-17, 2.736152283717910599E-16, -1.000000000000000000 ) ) ;
#11934 = CIRCLE ( 'NONE', #6131, 2.500000000000002220 ) ;
#11935 = ADVANCED_FACE ( 'NONE', ( #5045 ), #10310, .F. ) ;
#11936 = EDGE_LOOP ( 'NONE', ( #4144, #11766, #13520, #532 ) ) ;
#11937 = CYLINDRICAL_SURFACE ( 'NONE', #6279, 2.500000000000002220 ) ;
#11938 = CARTESIAN_POINT ( 'NONE',  ( 34.99999999999999289, 25.00000000000002132, 4.000000000000000000 ) ) ;
#11939 = EDGE_LOOP ( 'NONE', ( #4984, #5449, #2941, #8264 ) ) ;
#11940 = EDGE_CURVE ( 'NONE', #7842, #5381, #12923, .T. ) ;
#11941 = CARTESIAN_POINT ( 'NONE',  ( 31.93204061526060045, 3.910547132972217398E-15, 3.910547132972217398E-15 ) ) ;
#11942 = DIRECTION ( 'NONE',  ( -0.1234677578012386562, -1.701584941912606716E-18, 0.9923485843107423543 ) ) ;
#11943 = ORIENTED_EDGE ( 'NONE', *, *, #2849, .F. ) ;
#11944 = LINE ( 'NONE', #5633, #3921 ) ;
#11945 = ORIENTED_EDGE ( 'NONE', *, *, #6644, .F. ) ;
#11946 = DIRECTION ( 'NONE',  ( -0.000000000000000000, -0.000000000000000000, -1.000000000000000000 ) ) ;
#11947 = CARTESIAN_POINT ( 'NONE',  ( -10.69346802281035202, 2.474956373702985157, 21.38693604562069339 ) ) ;
#11948 = CIRCLE ( 'NONE', #9500, 79.99999999999997158 ) ;
#11949 = CARTESIAN_POINT ( 'NONE',  ( 21.12690199240172007, 12.61198448588842247, 2.500000000000002665 ) ) ;
#11950 = FACE_OUTER_BOUND ( 'NONE', #5157, .T. ) ;
#11951 = CARTESIAN_POINT ( 'NONE',  ( -35.00000000000000000, -35.00000000000000000, -4.000000000000000000 ) ) ;
#11952 = CARTESIAN_POINT ( 'NONE',  ( -15.29705854078140170, -29.33764382806072746, -1.769737219441121578E-15 ) ) ;
#11953 = CARTESIAN_POINT ( 'NONE',  ( -3.554095123023855901E-16, 12.70483462268159869, -2.243491919447391838E-17 ) ) ;
#11954 = CARTESIAN_POINT ( 'NONE',  ( -15.29705854078139282, 17.78624592198638155, 30.59411708156276788 ) ) ;
#11955 = B_SPLINE_CURVE_WITH_KNOTS ( 'NONE', 3,
 ( #6489, #185, #4661, #10886 ),
 .UNSPECIFIED., .F., .F.,
 ( 4, 4 ),
 ( 0.000000000000000000, 1.000000000000000000 ),
 .UNSPECIFIED. ) ;
#11956 = ORIENTED_EDGE ( 'NONE', *, *, #4051, .F. ) ;
#11957 = CIRCLE ( 'NONE', #7933, 16.99999999999998934 ) ;
#11958 = VERTEX_POINT ( 'NONE', #11750 ) ;
#11959 = DIRECTION ( 'NONE',  ( -2.797435172181481150E-17, 1.000000000000000000, -1.765856845898762549E-18 ) ) ;
#11960 = CARTESIAN_POINT ( 'NONE',  ( 0.000000000000000000, 0.000000000000000000, 0.000000000000000000 ) ) ;
#11961 = ORIENTED_EDGE ( 'NONE', *, *, #8437, .F. ) ;
#11962 = CARTESIAN_POINT ( 'NONE',  ( -10.69381717166375800, 25.55944687211528077, -1.399883545467522885E-15 ) ) ;
#11963 = CIRCLE ( 'NONE', #8602, 15.29705854078138927 ) ;
#11964 = CARTESIAN_POINT ( 'NONE',  ( -8.385254915620295790, 40.97916847270985130, -7.236334518677345233E-17 ) ) ;
#11965 = AXIS2_PLACEMENT_3D ( 'NONE', #11808, #1940, #2132 ) ;
#11966 = CARTESIAN_POINT ( 'NONE',  ( 0.000000000000000000, 71.01020514433645303, -2.499999999999998668 ) ) ;
#11967 = CARTESIAN_POINT ( 'NONE',  ( 25.00000000000000355, 120.0000000000000142, 2.499999999999999556 ) ) ;
#11968 = CIRCLE ( 'NONE', #2121, 14.99999999999999112 ) ;
#11969 = ORIENTED_EDGE ( 'NONE', *, *, #7775, .F. ) ;
#11970 = EDGE_LOOP ( 'NONE', ( #6927, #8473, #5901, #6373, #4101, #3948, #7556 ) ) ;
#11971 = LINE ( 'NONE', #11702, #2722 ) ;
#11972 = AXIS2_PLACEMENT_3D ( 'NONE', #13299, #2536, #7861 ) ;
#11973 = EDGE_LOOP ( 'NONE', ( #2506, #9767, #7124, #1290 ) ) ;
#11974 = DIRECTION ( 'NONE',  ( 2.797435172181480534E-17, -1.000000000000000000, 1.765856845898762164E-18 ) ) ;
#11975 = ORIENTED_EDGE ( 'NONE', *, *, #12447, .T. ) ;
#11976 = DIRECTION ( 'NONE',  ( -2.797435172181481150E-17, 1.000000000000000000, -1.765856845898762549E-18 ) ) ;
#11977 = AXIS2_PLACEMENT_3D ( 'NONE', #9001, #11245, #1631 ) ;
#11978 = EDGE_CURVE ( 'NONE', #1745, #7988, #8644, .T. ) ;
#11979 = CARTESIAN_POINT ( 'NONE',  ( 55.16425081158429577, -10.83695794929873912, -2.500000000000000000 ) ) ;
#11980 = PLANE ( 'NONE',  #13003 ) ;
#11981 = CARTESIAN_POINT ( 'NONE',  ( 35.00000000000000000, -4.286263797015736496E-15, -4.000000000000000000 ) ) ;
#11982 = DIRECTION ( 'NONE',  ( -1.000000000000000000, 0.000000000000000000, 0.000000000000000000 ) ) ;
#11983 = CARTESIAN_POINT ( 'NONE',  ( 25.00000000000000355, 120.0000000000000142, 2.500000000000000000 ) ) ;
#11984 = CARTESIAN_POINT ( 'NONE',  ( 34.99999999999958789, 1.091249486606660213E-13, 2.500000000000000000 ) ) ;
#11985 = AXIS2_PLACEMENT_3D ( 'NONE', #7951, #3883, #12306 ) ;
#11986 = ORIENTED_EDGE ( 'NONE', *, *, #12735, .F. ) ;
#11987 = DIRECTION ( 'NONE',  ( 0.9960067511297464593, -0.08927794634716622324, 3.401418580343279473E-17 ) ) ;
#11988 = ORIENTED_EDGE ( 'NONE', *, *, #1103, .F. ) ;
#11989 = TOROIDAL_SURFACE ( 'NONE', #6183, -34.24999999999974420, 69.24999999999975842 ) ;
#11990 = DIRECTION ( 'NONE',  ( -1.000000000000000000, 0.000000000000000000, 0.000000000000000000 ) ) ;
#11991 = DIRECTION ( 'NONE',  ( 6.158143864569485777E-17, 2.736152283717910599E-16, -1.000000000000000000 ) ) ;
#11992 = ORIENTED_EDGE ( 'NONE', *, *, #4228, .F. ) ;
#11993 = CARTESIAN_POINT ( 'NONE',  ( -10.00000000000000711, 92.00000000000000000, -2.500000000000000000 ) ) ;
#11994 = CIRCLE ( 'NONE', #5285, 4.999999999999997335 ) ;
#11995 = EDGE_CURVE ( 'NONE', #11418, #5860, #3270, .T. ) ;
#11996 = DIRECTION ( 'NONE',  ( 0.000000000000000000, 0.000000000000000000, 1.000000000000000000 ) ) ;
#11997 = CARTESIAN_POINT ( 'NONE',  ( -49.99999999999999289, 120.0000000000000284, 2.500000000000000000 ) ) ;
#11998 = ADVANCED_FACE ( 'NONE', ( #11289 ), #6354, .T. ) ;
#11999 = LINE ( 'NONE', #98, #11648 ) ;
#12000 = DIRECTION ( 'NONE',  ( 2.797435172181480534E-17, -1.000000000000000000, 1.765856845898762164E-18 ) ) ;
#12001 = EDGE_CURVE ( 'NONE', #4125, #5724, #8524, .T. ) ;
#12002 = CARTESIAN_POINT ( 'NONE',  ( 32.50000000000000000, 4.286263797015736496E-15, -4.000000000000000000 ) ) ;
#12003 = DIRECTION ( 'NONE',  ( 1.000000000000000000, 0.000000000000000000, 0.000000000000000000 ) ) ;
#12004 = EDGE_CURVE ( 'NONE', #13751, #3971, #8734, .T. ) ;
#12005 = SURFACE_STYLE_FILL_AREA ( #241 ) ;
#12006 = ADVANCED_FACE ( 'NONE', ( #261 ), #4377, .F. ) ;
#12007 = VERTEX_POINT ( 'NONE', #4441 ) ;
#12008 = ORIENTED_EDGE ( 'NONE', *, *, #12447, .F. ) ;
#12009 = DIRECTION ( 'NONE',  ( 0.000000000000000000, 0.000000000000000000, 1.000000000000000000 ) ) ;
#12010 = LINE ( 'NONE', #3244, #10297 ) ;
#12011 = ORIENTED_EDGE ( 'NONE', *, *, #3508, .F. ) ;
#12012 =( BOUNDED_SURFACE ( )  B_SPLINE_SURFACE ( 3, 3, ( 
 ( #13349, #2648, #6918, #11207 ),
 ( #565, #12333, #9106, #2724 ),
 ( #1671, #7130, #6020, #10563 ),
 ( #13698, #12682, #9513, #3062 ) ),
 .UNSPECIFIED., .F., .F., .T. ) 
 B_SPLINE_SURFACE_WITH_KNOTS ( ( 4, 4 ),
 ( 4, 4 ),
 ( 0.000000000000000000, 1.000000000000000000 ),
 ( 0.000000000000000000, 1.000000000000000000 ),
 .UNSPECIFIED. ) 
 GEOMETRIC_REPRESENTATION_ITEM ( )  RATIONAL_B_SPLINE_SURFACE ( (
 ( 1.000000000000000000, 0.3333333333333334259, 0.3333333333333334259, 1.000000000000000000),
 ( 1.000000000000000000, 0.3333333333333334259, 0.3333333333333334259, 1.000000000000000000),
 ( 1.000000000000000000, 0.3333333333333334259, 0.3333333333333334259, 1.000000000000000000),
 ( 1.000000000000000000, 0.3333333333333334259, 0.3333333333333334259, 1.000000000000000000) ) ) 
 REPRESENTATION_ITEM ( '' )  SURFACE ( )  );
#12013 = CARTESIAN_POINT ( 'NONE',  ( -23.64268088454699779, -97.00000000000000000, 0.000000000000000000 ) ) ;
#12014 = FACE_OUTER_BOUND ( 'NONE', #2046, .T. ) ;
#12015 = EDGE_LOOP ( 'NONE', ( #12879, #4556, #6897, #10949 ) ) ;
#12016 = LINE ( 'NONE', #2403, #1233 ) ;
#12017 = VERTEX_POINT ( 'NONE', #12025 ) ;
#12018 = CARTESIAN_POINT ( 'NONE',  ( 25.00000000000000355, 120.0000000000000142, -2.499999999999998668 ) ) ;
#12019 = CARTESIAN_POINT ( 'NONE',  ( -10.69381717166375800, 25.55944687211528077, -1.399883545467522885E-15 ) ) ;
#12020 = AXIS2_PLACEMENT_3D ( 'NONE', #12956, #3324, #11884 ) ;
#12021 = CARTESIAN_POINT ( 'NONE',  ( -25.00000000000000355, 120.0000000000000142, 0.5000000000000000000 ) ) ;
#12022 = DIRECTION ( 'NONE',  ( 0.9960067511297463483, -0.08927794634716618161, 4.818676322152979407E-17 ) ) ;
#12023 = DIRECTION ( 'NONE',  ( 1.000000000000000000, 0.000000000000000000, 0.000000000000000000 ) ) ;
#12024 = CARTESIAN_POINT ( 'NONE',  ( -40.81228451836347659, 100.6358150620708471, -0.5000000000000000000 ) ) ;
#12025 = CARTESIAN_POINT ( 'NONE',  ( 53.63671053572210923, -2.048907369402450218, -2.499999999999998224 ) ) ;
#12026 = EDGE_CURVE ( 'NONE', #7882, #13399, #10003, .T. ) ;
#12027 = CARTESIAN_POINT ( 'NONE',  ( -10.69346802281035202, 77.87317997377837742, -1.584597914529132607E-15 ) ) ;
#12028 = CARTESIAN_POINT ( 'NONE',  ( 8.385254915620297567, -6.144721277337255927, 1.036136684519089207E-15 ) ) ;
#12029 = ORIENTED_EDGE ( 'NONE', *, *, #9363, .F. ) ;
#12030 = ORIENTED_EDGE ( 'NONE', *, *, #571, .F. ) ;
#12031 = CARTESIAN_POINT ( 'NONE',  ( -35.45454545454546036, 140.4866414850956744, 2.500000000000000000 ) ) ;
#12032 = ORIENTED_EDGE ( 'NONE', *, *, #9712, .F. ) ;
#12033 = CARTESIAN_POINT ( 'NONE',  ( 47.16901142695026294, 17.29003067336574517, -2.499999999999993783 ) ) ;
#12034 =( NAMED_UNIT ( * ) PLANE_ANGLE_UNIT ( ) SI_UNIT ( $, .RADIAN. ) );
#12035 = ORIENTED_EDGE ( 'NONE', *, *, #6195, .T. ) ;
#12036 = DIRECTION ( 'NONE',  ( -0.000000000000000000, -0.000000000000000000, -1.000000000000000000 ) ) ;
#12037 = CARTESIAN_POINT ( 'NONE',  ( -12.99579180576517601, 54.65873172698324112, 25.99158361153033070 ) ) ;
#12038 = EDGE_CURVE ( 'NONE', #6322, #2621, #9735, .T. ) ;
#12039 = CARTESIAN_POINT ( 'NONE',  ( -35.00000000000000000, -4.286263797015736496E-15, 10.49999999999999822 ) ) ;
#12040 = CARTESIAN_POINT ( 'NONE',  ( 9.636121582682617870, -72.23759216827741625, 2.995460419705799904 ) ) ;
#12041 = ORIENTED_EDGE ( 'NONE', *, *, #7534, .T. ) ;
#12042 = VERTEX_POINT ( 'NONE', #12896 ) ;
#12043 = VECTOR ( 'NONE', #2661, 1000.000000000000000 ) ;
#12044 = ORIENTED_EDGE ( 'NONE', *, *, #10660, .T. ) ;
#12045 = ORIENTED_EDGE ( 'NONE', *, *, #11583, .F. ) ;
#12046 = CARTESIAN_POINT ( 'NONE',  ( 12.99579180576516713, 54.65873172698324112, 0.000000000000000000 ) ) ;
#12047 = EDGE_LOOP ( 'NONE', ( #2628, #5118, #10333, #8789 ) ) ;
#12048 = CARTESIAN_POINT ( 'NONE',  ( 35.65577094119244350, -20.24578327824959345, -2.500000000000003997 ) ) ;
#12049 = AXIS2_PLACEMENT_3D ( 'NONE', #1341, #13155, #3505 ) ;
#12050 = LINE ( 'NONE', #1129, #1086 ) ;
#12051 = LINE ( 'NONE', #4772, #12567 ) ;
#12052 = CIRCLE ( 'NONE', #8260, 48.00000000000001421 ) ;
#12053 = DIRECTION ( 'NONE',  ( 1.000000000000000000, 0.000000000000000000, 0.000000000000000000 ) ) ;
#12054 = CARTESIAN_POINT ( 'NONE',  ( 14.53672965213156942, 15.21527412409548674, 3.469446951953614189E-15 ) ) ;
#12055 = CARTESIAN_POINT ( 'NONE',  ( -1.698372594682201253, -102.6769990425255799, -7.133712067588741768 ) ) ;
#12056 = CARTESIAN_POINT ( 'NONE',  ( 9.857979974958242408, 4.257796268226282876, -2.499999999999999112 ) ) ;
#12057 = ORIENTED_EDGE ( 'NONE', *, *, #7140, .T. ) ;
#12058 = ORIENTED_EDGE ( 'NONE', *, *, #11677, .T. ) ;
#12059 = VERTEX_POINT ( 'NONE', #3392 ) ;
#12060 = ADVANCED_FACE ( 'NONE', ( #10961 ), #1237, .T. ) ;
#12061 = AXIS2_PLACEMENT_3D ( 'NONE', #10892, #11752, #5363 ) ;
#12062 = FACE_OUTER_BOUND ( 'NONE', #3407, .T. ) ;
#12063 = B_SPLINE_CURVE_WITH_KNOTS ( 'NONE', 3,
 ( #1197, #11912, #8553, #5460 ),
 .UNSPECIFIED., .F., .F.,
 ( 4, 4 ),
 ( 0.000000000000000000, 1.000000000000000000 ),
 .UNSPECIFIED. ) ;
#12064 = CARTESIAN_POINT ( 'NONE',  ( -25.00000000000000355, 120.0000000000000142, -2.499999999999998668 ) ) ;
#12065 = CIRCLE ( 'NONE', #6475, 9.000000000008999024 ) ;
#12066 = DIRECTION ( 'NONE',  ( -0.8735848310779960046, 0.4866719047884613403, 6.939263997980181797E-17 ) ) ;
#12067 = ORIENTED_EDGE ( 'NONE', *, *, #2924, .F. ) ;
#12068 = CARTESIAN_POINT ( 'NONE',  ( -10.69381717166375623, -2.714886977913000710, -1.300026693482923793E-15 ) ) ;
#12069 = CARTESIAN_POINT ( 'NONE',  ( -29.00000000000000355, -5.021051876504148963E-15, -10.49999999999999822 ) ) ;
#12070 = DIRECTION ( 'NONE',  ( -2.797435172181481150E-17, 1.000000000000000000, -1.765856845898762549E-18 ) ) ;
#12071 = DIRECTION ( 'NONE',  ( -0.000000000000000000, -0.000000000000000000, -1.000000000000000000 ) ) ;
#12072 = DIRECTION ( 'NONE',  ( 0.9960067511297464593, -0.08927794634716622324, 3.401418580343279473E-17 ) ) ;
#12073 = FACE_OUTER_BOUND ( 'NONE', #5826, .T. ) ;
#12074 = CARTESIAN_POINT ( 'NONE',  ( -1.410017725396658984E-15, 50.40394642271930792, -8.900615385087330109E-17 ) ) ;
#12075 = CIRCLE ( 'NONE', #3789, 15.29705854078138927 ) ;
#12076 = DIRECTION ( 'NONE',  ( 0.8907235428302444635, 0.4545454545454587492, 0.000000000000000000 ) ) ;
#12077 = DIRECTION ( 'NONE',  ( 0.9960067511297464593, -0.08927794634716622324, 6.802837160686558945E-17 ) ) ;
#12078 = VECTOR ( 'NONE', #13410, 1000.000000000000000 ) ;
#12079 = ORIENTED_EDGE ( 'NONE', *, *, #11820, .F. ) ;
#12080 = ADVANCED_FACE ( 'NONE', ( #10756 ), #127, .T. ) ;
#12081 = CARTESIAN_POINT ( 'NONE',  ( -2.517691654963332357E-15, 90.00000000000000000, -1.589271161308885878E-16 ) ) ;
#12082 = EDGE_CURVE ( 'NONE', #5463, #6752, #5737, .T. ) ;
#12083 = CARTESIAN_POINT ( 'NONE',  ( 17.19653809941365452, 5.878923826270380459, 2.500000000000000444 ) ) ;
#12084 = AXIS2_PLACEMENT_3D ( 'NONE', #8369, #6268, #10540 ) ;
#12085 = ADVANCED_FACE ( 'NONE', ( #188 ), #2263, .T. ) ;
#12086 = ORIENTED_EDGE ( 'NONE', *, *, #10858, .F. ) ;
#12087 = ORIENTED_EDGE ( 'NONE', *, *, #8399, .T. ) ;
#12088 = CARTESIAN_POINT ( 'NONE',  ( -37.50000000000000000, 120.0000000000000142, 7.500000000000000000 ) ) ;
#12089 = ORIENTED_EDGE ( 'NONE', *, *, #11665, .F. ) ;
#12090 = ADVANCED_FACE ( 'NONE', ( #7812 ), #4814, .T. ) ;
#12091 = DIRECTION ( 'NONE',  ( 0.4206864060305147146, -0.9072061219927526343, -2.313087999326727677E-16 ) ) ;
#12092 = AXIS2_PLACEMENT_3D ( 'NONE', #12081, #2551, #13092 ) ;
#12093 = CIRCLE ( 'NONE', #7, 15.29705854078139460 ) ;
#12094 = CARTESIAN_POINT ( 'NONE',  ( 4.961407659643947810, 90.00000000000001421, -0.6346170828971222644 ) ) ;
#12095 = CARTESIAN_POINT ( 'NONE',  ( 2.406219558548489190E-16, -8.601520358636511432, 1.518905361043589440E-17 ) ) ;
#12096 = DIRECTION ( 'NONE',  ( 0.000000000000000000, 0.000000000000000000, 1.000000000000000000 ) ) ;
#12097 = CARTESIAN_POINT ( 'NONE',  ( 35.00000000000000000, -4.286263797015736496E-15, 4.000000000000000000 ) ) ;
#12098 = CARTESIAN_POINT ( 'NONE',  ( -10.11144051725924520, -69.99977036137985920, 0.2534939247371171822 ) ) ;
#12099 = CARTESIAN_POINT ( 'NONE',  ( -12.99579180576517778, -30.16426982310158422, 25.99158361153034136 ) ) ;
#12100 = LINE ( 'NONE', #1509, #4526 ) ;
#12101 = CARTESIAN_POINT ( 'NONE',  ( -8.385254915620294014, -6.144721277337256815, -16.77050983124059513 ) ) ;
#12102 = CIRCLE ( 'NONE', #9427, 15.29705854078140170 ) ;
#12103 = ADVANCED_FACE ( 'NONE', ( #10209 ), #9517, .T. ) ;
#12104 = ORIENTED_EDGE ( 'NONE', *, *, #7396, .F. ) ;
#12105 = AXIS2_PLACEMENT_3D ( 'NONE', #10199, #5859, #9080 ) ;
#12106 = ORIENTED_EDGE ( 'NONE', *, *, #7873, .F. ) ;
#12107 = EDGE_CURVE ( 'NONE', #1315, #1460, #10146, .T. ) ;
#12108 = ORIENTED_EDGE ( 'NONE', *, *, #13252, .T. ) ;
#12109 = ADVANCED_FACE ( 'NONE', ( #8038 ), #1658, .T. ) ;
#12110 = DIRECTION ( 'NONE',  ( 0.9063077870366492705, 0.4226182617407009956, 0.000000000000000000 ) ) ;
#12111 = AXIS2_PLACEMENT_3D ( 'NONE', #2871, #7212, #11563 ) ;
#12112 = DIRECTION ( 'NONE',  ( 0.000000000000000000, 0.000000000000000000, 1.000000000000000000 ) ) ;
#12113 = ORIENTED_EDGE ( 'NONE', *, *, #8153, .F. ) ;
#12114 = LINE ( 'NONE', #3620, #12661 ) ;
#12115 = AXIS2_PLACEMENT_3D ( 'NONE', #2440, #7495, #1060 ) ;
#12116 = VECTOR ( 'NONE', #6376, 1000.000000000000000 ) ;
#12117 = CARTESIAN_POINT ( 'NONE',  ( -35.00000000000000000, -4.286263797015736496E-15, -7.500000000000000000 ) ) ;
#12118 = CARTESIAN_POINT ( 'NONE',  ( 50.00000000000000000, 120.0000000000000142, 0.5000000000000000000 ) ) ;
#12119 = CARTESIAN_POINT ( 'NONE',  ( 9.876538003337365978, -71.62961015055314817, 2.126563534463134619 ) ) ;
#12120 = ORIENTED_EDGE ( 'NONE', *, *, #8833, .T. ) ;
#12121 = SURFACE_STYLE_USAGE ( .BOTH. , #2514 ) ;
#12122 = ORIENTED_EDGE ( 'NONE', *, *, #11663, .T. ) ;
#12123 = EDGE_CURVE ( 'NONE', #3017, #1421, #3729, .T. ) ;
#12124 = VECTOR ( 'NONE', #2838, 1000.000000000000000 ) ;
#12125 = ORIENTED_EDGE ( 'NONE', *, *, #12304, .T. ) ;
#12126 = AXIS2_PLACEMENT_3D ( 'NONE', #3180, #6414, #7190 ) ;
#12127 = DIRECTION ( 'NONE',  ( -0.6000000000000001998, -0.7999999999999998224, 0.000000000000000000 ) ) ;
#12128 = EDGE_CURVE ( 'NONE', #2483, #3335, #829, .T. ) ;
#12129 = ORIENTED_EDGE ( 'NONE', *, *, #1669, .T. ) ;
#12130 = ORIENTED_EDGE ( 'NONE', *, *, #2795, .T. ) ;
#12131 = FILL_AREA_STYLE ('',( #10168 ) ) ;
#12132 = CARTESIAN_POINT ( 'NONE',  ( 15.29705854078138749, 76.22148119144830503, 3.746698755667522411E-15 ) ) ;
#12133 = CARTESIAN_POINT ( 'NONE',  ( 19.38529118556630237, 26.86594603178324903, -5.082853661574512572 ) ) ;
#12134 = AXIS2_PLACEMENT_3D ( 'NONE', #4270, #13193, #3540 ) ;
#12135 = DIRECTION ( 'NONE',  ( -0.000000000000000000, -0.000000000000000000, -1.000000000000000000 ) ) ;
#12136 = LINE ( 'NONE', #4476, #1872 ) ;
#12137 = FACE_OUTER_BOUND ( 'NONE', #1679, .T. ) ;
#12138 = ORIENTED_EDGE ( 'NONE', *, *, #6375, .F. ) ;
#12139 = ORIENTED_EDGE ( 'NONE', *, *, #9381, .F. ) ;
#12140 = CARTESIAN_POINT ( 'NONE',  ( -8.567019981000800755, -91.60288616555511965, -1.484956459547787544 ) ) ;
#12141 = CIRCLE ( 'NONE', #6106, 2.500000000000000444 ) ;
#12142 = FACE_OUTER_BOUND ( 'NONE', #9374, .T. ) ;
#12143 = CARTESIAN_POINT ( 'NONE',  ( -1.024078386997803625, -80.66666666666729668, 9.976024522091169189 ) ) ;
#12144 = ORIENTED_EDGE ( 'NONE', *, *, #10365, .T. ) ;
#12145 = CARTESIAN_POINT ( 'NONE',  ( 4.330127018922196314, 91.72908881866754882, 2.499999999999993783 ) ) ;
#12146 = CARTESIAN_POINT ( 'NONE',  ( -35.00000000000000000, -4.286263797015736496E-15, -10.49999999999999822 ) ) ;
#12147 = CARTESIAN_POINT ( 'NONE',  ( 27.98552063842490867, -17.38741154648219833, -2.500000000000004441 ) ) ;
#12148 = PLANE ( 'NONE',  #13888 ) ;
#12149 = CARTESIAN_POINT ( 'NONE',  ( 0.2890385494233890795, -128.7272727272696500, -4.499839249777167538 ) ) ;
#12150 = CARTESIAN_POINT ( 'NONE',  ( 1.958204620527036497E-15, -70.00000000000000000, 1.236099792129133461E-16 ) ) ;
#12151 = DIRECTION ( 'NONE',  ( -6.158143864569485777E-17, -2.736152283717910599E-16, 1.000000000000000000 ) ) ;
#12152 = DIRECTION ( 'NONE',  ( 0.6000000000000001998, 0.7999999999999999334, 0.000000000000000000 ) ) ;
#12153 = EDGE_LOOP ( 'NONE', ( #3856, #13159, #11212, #5569 ) ) ;
#12154 = EDGE_LOOP ( 'NONE', ( #13020, #7137, #10596, #2677 ) ) ;
#12155 = ORIENTED_EDGE ( 'NONE', *, *, #6984, .F. ) ;
#12156 = CARTESIAN_POINT ( 'NONE',  ( 0.5086153989323403124, -157.9221515666981190, 1.416975838558779177 ) ) ;
#12157 = VERTEX_POINT ( 'NONE', #5715 ) ;
#12158 = DIRECTION ( 'NONE',  ( 0.000000000000000000, 0.000000000000000000, 1.000000000000000000 ) ) ;
#12159 = DIRECTION ( 'NONE',  ( -6.158143864569485777E-17, -2.736152283717910599E-16, 1.000000000000000000 ) ) ;
#12160 = CARTESIAN_POINT ( 'NONE',  ( 34.66997162884352690, 21.14050806081579736, -2.499999999999992895 ) ) ;
#12161 = CARTESIAN_POINT ( 'NONE',  ( -8.385254915620292238, 79.99058638175036151, -1.412519245696701158E-16 ) ) ;
#12162 = VERTEX_POINT ( 'NONE', #2843 ) ;
#12163 = AXIS2_PLACEMENT_3D ( 'NONE', #5166, #3910, #2857 ) ;
#12164 = ORIENTED_EDGE ( 'NONE', *, *, #9467, .F. ) ;
#12165 = CARTESIAN_POINT ( 'NONE',  ( 10.00024727050385920, -5.026167870790866132, 2.499999999999996891 ) ) ;
#12166 = EDGE_LOOP ( 'NONE', ( #5942, #7070, #9900, #10527, #10842, #2161, #5759, #13097 ) ) ;
#12167 = DIRECTION ( 'NONE',  ( -0.4545454545454531425, -0.8907235428302472391, 0.000000000000000000 ) ) ;
#12168 = CARTESIAN_POINT ( 'NONE',  ( -10.69381717166375090, 44.40900277213413716, -21.38763434332750890 ) ) ;
#12169 = CARTESIAN_POINT ( 'NONE',  ( 26.79177319725820539, -26.24642857144861807, 4.000000000000000000 ) ) ;
#12170 = ADVANCED_FACE ( 'NONE', ( #1723, #11265 ), #1582, .T. ) ;
#12171 = LINE ( 'NONE', #6903, #5980 ) ;
#12172 = CARTESIAN_POINT ( 'NONE',  ( -10.10544246792081857, -70.44230941534301849, -0.3214603539705591650 ) ) ;
#12173 = EDGE_CURVE ( 'NONE', #9444, #10078, #11390, .T. ) ;
#12174 = CARTESIAN_POINT ( 'NONE',  ( -8.385254915620294014, 90.00000000000000000, -1.589271161308885878E-16 ) ) ;
#12175 = DIRECTION ( 'NONE',  ( 1.000000000000000000, 0.000000000000000000, -0.000000000000000000 ) ) ;
#12176 = VECTOR ( 'NONE', #2238, 1000.000000000000000 ) ;
#12177 = DIRECTION ( 'NONE',  ( -0.9961946980917455452, -0.08715574274765884588, 0.000000000000000000 ) ) ;
#12178 = ORIENTED_EDGE ( 'NONE', *, *, #1082, .T. ) ;
#12179 = CARTESIAN_POINT ( 'NONE',  ( -6.733243228433030581, -82.89610389607871355, 12.92256141468849506 ) ) ;
#12180 = VECTOR ( 'NONE', #1550, 1000.000000000000000 ) ;
#12181 = ORIENTED_EDGE ( 'NONE', *, *, #10772, .F. ) ;
#12182 =( GEOMETRIC_REPRESENTATION_CONTEXT ( 3 ) GLOBAL_UNCERTAINTY_ASSIGNED_CONTEXT ( ( #7133 ) ) GLOBAL_UNIT_ASSIGNED_CONTEXT ( ( #2760, #11304, #9209 ) ) REPRESENTATION_CONTEXT ( 'NONE', 'WORKASPACE' ) );
#12183 = CARTESIAN_POINT ( 'NONE',  ( 8.385254915620292238, 50.40394642271930792, 9.355740606675297531E-16 ) ) ;
#12184 = APPLICATION_PROTOCOL_DEFINITION ( 'draft international standard', 'automotive_design', 1998, #7010 ) ;
#12185 = ORIENTED_EDGE ( 'NONE', *, *, #275, .T. ) ;
#12186 = DIRECTION ( 'NONE',  ( 1.000000000000000000, 0.000000000000000000, 0.000000000000000000 ) ) ;
#12187 = ADVANCED_FACE ( 'NONE', ( #4877 ), #9154, .T. ) ;
#12188 = DIRECTION ( 'NONE',  ( 0.000000000000000000, 0.000000000000000000, -1.000000000000000000 ) ) ;
#12189 = ADVANCED_FACE ( 'NONE', ( #6009 ), #6843, .F. ) ;
#12190 = EDGE_CURVE ( 'NONE', #9797, #1472, #3060, .T. ) ;
#12191 = DIRECTION ( 'NONE',  ( -2.797435172181481150E-17, 1.000000000000000000, -1.765856845898762549E-18 ) ) ;
#12192 = CARTESIAN_POINT ( 'NONE',  ( 7.128864087426364016, -75.84752376712806665, 7.199434346136632357 ) ) ;
#12193 = EDGE_CURVE ( 'NONE', #8713, #12944, #2550, .T. ) ;
#12194 = VECTOR ( 'NONE', #720, 1000.000000000000000 ) ;
#12195 = ORIENTED_EDGE ( 'NONE', *, *, #6531, .T. ) ;
#12196 = EDGE_CURVE ( 'NONE', #12494, #1107, #7687, .T. ) ;
#12197 = CARTESIAN_POINT ( 'NONE',  ( 25.00000000000000355, 120.0000000000000142, -0.5000000000000000000 ) ) ;
#12198 = ORIENTED_EDGE ( 'NONE', *, *, #2852, .F. ) ;
#12199 = CARTESIAN_POINT ( 'NONE',  ( 12.99553232110415024, -26.62435705548576692, -25.99106464220828627 ) ) ;
#12200 = AXIS2_PLACEMENT_3D ( 'NONE', #5176, #3069, #7335 ) ;
#12201 = ORIENTED_EDGE ( 'NONE', *, *, #7551, .F. ) ;
#12202 = EDGE_LOOP ( 'NONE', ( #9862, #272, #9276, #9355 ) ) ;
#12203 = DIRECTION ( 'NONE',  ( -1.000000000000000000, 0.000000000000000000, 0.000000000000000000 ) ) ;
#12204 = AXIS2_PLACEMENT_3D ( 'NONE', #13821, #8385, #11544 ) ;
#12205 = DIRECTION ( 'NONE',  ( 0.000000000000000000, 0.000000000000000000, -1.000000000000000000 ) ) ;
#12206 = ADVANCED_FACE ( 'NONE', ( #8373 ), #7022, .T. ) ;
#12207 = CIRCLE ( 'NONE', #13829, 20.00000000000000000 ) ;
#12208 = CARTESIAN_POINT ( 'NONE',  ( -10.69381717166375623, 34.98422482212468054, -1.433169162795722386E-15 ) ) ;
#12209 = CARTESIAN_POINT ( 'NONE',  ( -34.25812584745457201, 108.1980041606220908, 0.6234749816336021544 ) ) ;
#12210 = CARTESIAN_POINT ( 'NONE',  ( -1.520893302047029660, -106.0215521432844952, 6.750146769911295586 ) ) ;
#12211 = CARTESIAN_POINT ( 'NONE',  ( -8.385254915620292238, 15.32944684068712782, -2.089804632053991565E-15 ) ) ;
#12212 = VERTEX_POINT ( 'NONE', #12807 ) ;
#12213 = EDGE_CURVE ( 'NONE', #1501, #2348, #6145, .T. ) ;
#12214 = ORIENTED_EDGE ( 'NONE', *, *, #12957, .T. ) ;
#12215 = CIRCLE ( 'NONE', #10629, 9.000000000009000800 ) ;
#12216 = AXIS2_PLACEMENT_3D ( 'NONE', #4167, #403, #9013 ) ;
#12217 = ORIENTED_EDGE ( 'NONE', *, *, #2673, .T. ) ;
#12218 = LINE ( 'NONE', #10245, #13108 ) ;
#12219 = CARTESIAN_POINT ( 'NONE',  ( 9.807291687912153222, -69.33333333333652604, 2.012068907120017514 ) ) ;
#12220 = ORIENTED_EDGE ( 'NONE', *, *, #1045, .T. ) ;
#12221 = DIRECTION ( 'NONE',  ( 0.000000000000000000, 0.000000000000000000, 1.000000000000000000 ) ) ;
#12222 = PRESENTATION_STYLE_ASSIGNMENT (( #591 ) ) ;
#12223 = CARTESIAN_POINT ( 'NONE',  ( 10.69346802281034847, -35.22415542633469698, 0.000000000000000000 ) ) ;
#12224 = DIRECTION ( 'NONE',  ( 0.9960067511297463483, -0.08927794634716620936, 4.626175998653454121E-17 ) ) ;
#12225 = CARTESIAN_POINT ( 'NONE',  ( -34.25812584745457201, 108.1980041606221192, -0.5000000000000000000 ) ) ;
#12226 = CARTESIAN_POINT ( 'NONE',  ( 2.739930038170992344, -137.4545454545608720, 2.373837707219488280 ) ) ;
#12227 = DIRECTION ( 'NONE',  ( -1.000000000000000000, -1.224646799147353207E-16, 0.000000000000000000 ) ) ;
#12228 = CARTESIAN_POINT ( 'NONE',  ( 15.47908363509431595, -16.40738050097609602, 2.711248065311635091 ) ) ;
#12229 =( GEOMETRIC_REPRESENTATION_CONTEXT ( 3 ) GLOBAL_UNCERTAINTY_ASSIGNED_CONTEXT ( ( #4763 ) ) GLOBAL_UNIT_ASSIGNED_CONTEXT ( ( #7860, #1207, #4491 ) ) REPRESENTATION_CONTEXT ( 'NONE', 'WORKASPACE' ) );
#12230 = FACE_OUTER_BOUND ( 'NONE', #1548, .T. ) ;
#12231 = ORIENTED_EDGE ( 'NONE', *, *, #7825, .T. ) ;
#12232 = ORIENTED_EDGE ( 'NONE', *, *, #1283, .F. ) ;
#12233 = DIRECTION ( 'NONE',  ( -1.000000000000000000, 0.000000000000000000, 0.000000000000000000 ) ) ;
#12234 = EDGE_LOOP ( 'NONE', ( #12963, #2674, #2030, #11021 ) ) ;
#12235 = CARTESIAN_POINT ( 'NONE',  ( 0.7709178830051971465, -102.1536708361958716, -7.353836487445167158 ) ) ;
#12236 = ADVANCED_FACE ( 'NONE', ( #10609 ), #13854, .T. ) ;
#12237 = CIRCLE ( 'NONE', #5063, 15.29705854078139105 ) ;
#12238 = LINE ( 'NONE', #13535, #5273 ) ;
#12239 = DIRECTION ( 'NONE',  ( -0.9462100554738961389, -0.3235529800822216639, -1.445602896645893329E-16 ) ) ;
#12240 = VERTEX_POINT ( 'NONE', #11668 ) ;
#12241 = FACE_OUTER_BOUND ( 'NONE', #5132, .T. ) ;
#12242 = ORIENTED_EDGE ( 'NONE', *, *, #6870, .T. ) ;
#12243 = TOROIDAL_SURFACE ( 'NONE', #13580, 22.49999999999999289, 5.000000000000000000 ) ;
#12244 = DIRECTION ( 'NONE',  ( -0.7328050451781165098, -0.6804386568688601811, -2.409338161076489210E-16 ) ) ;
#12245 = DIRECTION ( 'NONE',  ( 1.000000000000000000, 0.000000000000000000, 1.224646799147352961E-16 ) ) ;
#12246 = DIRECTION ( 'NONE',  ( 0.000000000000000000, 1.000000000000000000, 0.000000000000000000 ) ) ;
#12247 = CARTESIAN_POINT ( 'NONE',  ( 35.06230589874905945, 106.5835921350012825, 2.486789939184904874 ) ) ;
#12248 = DIRECTION ( 'NONE',  ( -1.000000000000000000, 0.000000000000000000, 0.000000000000000000 ) ) ;
#12249 = CARTESIAN_POINT ( 'NONE',  ( 12.99553232110414669, -26.62435705548577047, 0.000000000000000000 ) ) ;
#12250 = AXIS2_PLACEMENT_3D ( 'NONE', #10625, #5299, #1033 ) ;
#12251 = FACE_OUTER_BOUND ( 'NONE', #7082, .T. ) ;
#12252 = ORIENTED_EDGE ( 'NONE', *, *, #480, .T. ) ;
#12253 = ORIENTED_EDGE ( 'NONE', *, *, #2304, .T. ) ;
#12254 = CARTESIAN_POINT ( 'NONE',  ( 2.940534136604410875, -72.18181818207969513, 3.082537950474903088 ) ) ;
#12255 = EDGE_CURVE ( 'NONE', #7855, #3210, #3907, .T. ) ;
#12256 = AXIS2_PLACEMENT_3D ( 'NONE', #1601, #8122, #5729 ) ;
#12257 = ORIENTED_EDGE ( 'NONE', *, *, #2888, .T. ) ;
#12258 = CARTESIAN_POINT ( 'NONE',  ( 0.000000000000000000, -20.00000000000000000, 0.000000000000000000 ) ) ;
#12259 = CARTESIAN_POINT ( 'NONE',  ( 6.733243228435068950, -82.89610389607662455, -12.92256141468959640 ) ) ;
#12260 = CARTESIAN_POINT ( 'NONE',  ( 12.99579180576516535, 7.534841976936129448, 3.183050967463141802E-15 ) ) ;
#12261 = DIRECTION ( 'NONE',  ( -0.000000000000000000, -0.000000000000000000, 1.000000000000000000 ) ) ;
#12262 = CARTESIAN_POINT ( 'NONE',  ( 10.69346802281033781, 21.32451227372186864, 21.38693604562068629 ) ) ;
#12263 = CARTESIAN_POINT ( 'NONE',  ( 14.13596196814456718, -39.17949320881311337, 28.27192393628914502 ) ) ;
#12264 = EDGE_LOOP ( 'NONE', ( #6729, #2250, #8275, #10945 ) ) ;
#12265 = ORIENTED_EDGE ( 'NONE', *, *, #966, .F. ) ;
#12266 = ADVANCED_FACE ( 'NONE', ( #8443 ), #12731, .F. ) ;
#12267 = FACE_OUTER_BOUND ( 'NONE', #4601, .T. ) ;
#12268 = EDGE_LOOP ( 'NONE', ( #6246, #7691, #3212, #1185 ) ) ;
#12269 = VERTEX_POINT ( 'NONE', #10349 ) ;
#12270 = ORIENTED_EDGE ( 'NONE', *, *, #2697, .T. ) ;
#12271 = EDGE_CURVE ( 'NONE', #9210, #3082, #3208, .T. ) ;
#12272 = CARTESIAN_POINT ( 'NONE',  ( -15.29705854078138394, -36.87585420866476937, -30.59411708156277854 ) ) ;
#12273 = EDGE_CURVE ( 'NONE', #2573, #4214, #11948, .T. ) ;
#12274 = CARTESIAN_POINT ( 'NONE',  ( -9.357262989153291244, -70.83714849354491605, -3.840749687708657767 ) ) ;
#12275 = CARTESIAN_POINT ( 'NONE',  ( 10.00000000000000711, 139.9999999999999716, 0.5000000000000000000 ) ) ;
#12276 = CARTESIAN_POINT ( 'NONE',  ( 8.182234252389633866, -94.33801111161687913, 1.656266771341373900 ) ) ;
#12277 = CARTESIAN_POINT ( 'NONE',  ( 32.95454545454548878, 135.5876619995293026, -7.500000000000000000 ) ) ;
#12278 = ORIENTED_EDGE ( 'NONE', *, *, #10243, .F. ) ;
#12279 = EDGE_LOOP ( 'NONE', ( #4112, #4836, #11001, #6010, #3992, #22, #12576, #2264, #3857, #7029 ) ) ;
#12280 = ORIENTED_EDGE ( 'NONE', *, *, #6515, .T. ) ;
#12281 = DIRECTION ( 'NONE',  ( -2.797435172181481150E-17, 1.000000000000000000, -1.765856845898762549E-18 ) ) ;
#12282 = ORIENTED_EDGE ( 'NONE', *, *, #4629, .F. ) ;
#12283 = DIRECTION ( 'NONE',  ( 0.000000000000000000, 0.000000000000000000, 1.000000000000000000 ) ) ;
#12284 = AXIS2_PLACEMENT_3D ( 'NONE', #6819, #1556, #5846 ) ;
#12285 = CARTESIAN_POINT ( 'NONE',  ( -1.463793564954975146, -80.12121212121181202, 10.07802918118912139 ) ) ;
#12286 = ORIENTED_EDGE ( 'NONE', *, *, #13832, .T. ) ;
#12287 = CARTESIAN_POINT ( 'NONE',  ( 15.29705854078140170, -19.91286587805129926, 1.906846944237140710E-15 ) ) ;
#12288 =( NAMED_UNIT ( * ) SI_UNIT ( $, .STERADIAN. ) SOLID_ANGLE_UNIT ( ) );
#12289 = ADVANCED_FACE ( 'NONE', ( #7317 ), #13786, .T. ) ;
#12290 = DIRECTION ( 'NONE',  ( 0.9923485843107423543, 2.797833471351478217E-17, 0.1234677578012386562 ) ) ;
#12291 = CARTESIAN_POINT ( 'NONE',  ( 4.855892414095402287, -117.0909090909090793, 4.610765637404218076 ) ) ;
#12292 = CARTESIAN_POINT ( 'NONE',  ( -12.99579180576517068, 45.23395377697383424, 25.99158361153032004 ) ) ;
#12293 = CARTESIAN_POINT ( 'NONE',  ( -4.418010223188907126, -106.9090909090898549, 5.547116815809651769 ) ) ;
#12294 = DIRECTION ( 'NONE',  ( 1.000000000000000000, 0.000000000000000000, 0.000000000000000000 ) ) ;
#12295 = CARTESIAN_POINT ( 'NONE',  ( -32.72727272727271952, 135.1423002281142089, -0.5000000000000000000 ) ) ;
#12296 = DIRECTION ( 'NONE',  ( 0.000000000000000000, 1.000000000000000000, 0.000000000000000000 ) ) ;
#12297 = ORIENTED_EDGE ( 'NONE', *, *, #9112, .T. ) ;
#12298 = EDGE_LOOP ( 'NONE', ( #3467, #9416, #12771 ) ) ;
#12299 = AXIS2_PLACEMENT_3D ( 'NONE', #1945, #9515, #9245 ) ;
#12300 = CARTESIAN_POINT ( 'NONE',  ( 1.146825886634105895, -155.8473912411174354, 1.122800904668010302 ) ) ;
#12301 = ORIENTED_EDGE ( 'NONE', *, *, #2304, .F. ) ;
#12302 = CARTESIAN_POINT ( 'NONE',  ( -5.052187264070409967, -96.66555973379486488, -6.278296762411313736 ) ) ;
#12303 =( REPRESENTATION_RELATIONSHIP ('NONE','NONE', #9450, #2342 ) REPRESENTATION_RELATIONSHIP_WITH_TRANSFORMATION ( #5802 )SHAPE_REPRESENTATION_RELATIONSHIP( ) );
#12304 = EDGE_CURVE ( 'NONE', #11415, #4734, #10091, .T. ) ;
#12305 = DIRECTION ( 'NONE',  ( -6.158143864569485777E-17, -2.736152283717910599E-16, 1.000000000000000000 ) ) ;
#12306 = DIRECTION ( 'NONE',  ( 1.000000000000000000, 0.000000000000000000, 0.000000000000000000 ) ) ;
#12307 = CARTESIAN_POINT ( 'NONE',  ( 42.70768697973989703, 17.09141780026012469, 2.500000000000005329 ) ) ;
#12308 = DIRECTION ( 'NONE',  ( -1.000000000000000000, 0.000000000000000000, 0.000000000000000000 ) ) ;
#12309 = DIRECTION ( 'NONE',  ( 0.000000000000000000, 0.000000000000000000, -1.000000000000000000 ) ) ;
#12310 = DIRECTION ( 'NONE',  ( -6.158143864569485777E-17, -2.736152283717910599E-16, 1.000000000000000000 ) ) ;
#12311 = ADVANCED_FACE ( 'NONE', ( #10475 ), #12669, .T. ) ;
#12312 = VECTOR ( 'NONE', #10601, 1000.000000000000000 ) ;
#12313 = DIRECTION ( 'NONE',  ( 0.000000000000000000, 0.000000000000000000, 1.000000000000000000 ) ) ;
#12314 = FACE_OUTER_BOUND ( 'NONE', #2314, .T. ) ;
#12315 = CARTESIAN_POINT ( 'NONE',  ( 34.06230589874904524, 109.5835921350012683, 2.499999999999999556 ) ) ;
#12316 = CARTESIAN_POINT ( 'NONE',  ( -15.29705854078140170, -29.33764382806072746, 5.180607919632063331E-17 ) ) ;
#12317 = CARTESIAN_POINT ( 'NONE',  ( 1.958204620527036497E-15, -70.00000000000000000, 1.236099792129133461E-16 ) ) ;
#12318 = SHAPE_REPRESENTATION ( 'Dual Pivoting Lever Wings (x2)', ( #8193 ), #5278 ) ;
#12319 = CARTESIAN_POINT ( 'NONE',  ( -10.69381717166375800, 63.25855867215300066, 21.38763434332750535 ) ) ;
#12320 = CARTESIAN_POINT ( 'NONE',  ( 8.385254915620292238, 40.97916847270985130, 9.522168693316296019E-16 ) ) ;
#12321 = AXIS2_PLACEMENT_3D ( 'NONE', #12597, #5081, #2056 ) ;
#12322 = EDGE_LOOP ( 'NONE', ( #10631, #2913, #11, #10852 ) ) ;
#12323 = CARTESIAN_POINT ( 'NONE',  ( 2.886819890957835977, -105.1818181818214128, -3.599275682873738003 ) ) ;
#12324 = VERTEX_POINT ( 'NONE', #1993 ) ;
#12325 = AXIS2_PLACEMENT_3D ( 'NONE', #5286, #13682, #8377 ) ;
#12326 = ORIENTED_EDGE ( 'NONE', *, *, #12255, .F. ) ;
#12327 = DIRECTION ( 'NONE',  ( 0.000000000000000000, 0.000000000000000000, 1.000000000000000000 ) ) ;
#12328 = FACE_OUTER_BOUND ( 'NONE', #3757, .T. ) ;
#12329 = CONTEXT_DEPENDENT_SHAPE_REPRESENTATION ( #760, #5755 ) ;
#12330 = CARTESIAN_POINT ( 'NONE',  ( -1.275238607045734884, -147.1038961039145647, 4.986937111402549583 ) ) ;
#12331 = STYLED_ITEM ( 'NONE', ( #8550 ), #7695 ) ;
#12332 = CARTESIAN_POINT ( 'NONE',  ( -8.385254915620294014, 5.904668890677672088, 16.77050983124058092 ) ) ;
#12333 = CARTESIAN_POINT ( 'NONE',  ( -12.99579180576517601, -20.73949187309215247, 25.99158361153034136 ) ) ;
#12334 = AXIS2_PLACEMENT_3D ( 'NONE', #9769, #2473, #8937 ) ;
#12335 = CARTESIAN_POINT ( 'NONE',  ( -12.99553232110414491, -36.04913500549519512, 25.99106464220827917 ) ) ;
#12336 = EDGE_CURVE ( 'NONE', #11003, #4722, #1665, .T. ) ;
#12337 = AXIS2_PLACEMENT_3D ( 'NONE', #7662, #4505, #10810 ) ;
#12338 = PRODUCT_DEFINITION_CONTEXT ( 'detailed design', #7010, 'design' ) ;
#12339 = CARTESIAN_POINT ( 'NONE',  ( 5.799822717052470544, -77.11029875732677397, 8.314269019852831732 ) ) ;
#12340 = ORIENTED_EDGE ( 'NONE', *, *, #139, .T. ) ;
#12341 = EDGE_LOOP ( 'NONE', ( #7657, #4319 ) ) ;
#12342 = AXIS2_PLACEMENT_3D ( 'NONE', #13611, #1581, #2635 ) ;
#12343 = CARTESIAN_POINT ( 'NONE',  ( -10.69346802281034670, -25.79937747632526879, -2.581358761202454000E-15 ) ) ;
#12344 = AXIS2_PLACEMENT_3D ( 'NONE', #762, #5028, #9382 ) ;
#12345 = AXIS2_PLACEMENT_3D ( 'NONE', #5999, #2771, #12239 ) ;
#12346 = ORIENTED_EDGE ( 'NONE', *, *, #6112, .T. ) ;
#12347 = ORIENTED_EDGE ( 'NONE', *, *, #5247, .F. ) ;
#12348 = FACE_OUTER_BOUND ( 'NONE', #9111, .T. ) ;
#12349 = CARTESIAN_POINT ( 'NONE',  ( -15.29705854078139282, -8.601520358636511432, 1.518905361043589440E-17 ) ) ;
#12350 = CARTESIAN_POINT ( 'NONE',  ( -9.704377265674031250, -70.11112484213649054, -2.862656033565787794 ) ) ;
#12351 = DIRECTION ( 'NONE',  ( 0.000000000000000000, 0.000000000000000000, 1.000000000000000000 ) ) ;
#12352 = CARTESIAN_POINT ( 'NONE',  ( 1.395779086812880765, -82.48867648896566607, -9.636429481739551051 ) ) ;
#12353 = EDGE_CURVE ( 'NONE', #9880, #4466, #4800, .T. ) ;
#12354 = VECTOR ( 'NONE', #7518, 1000.000000000000000 ) ;
#12355 = CARTESIAN_POINT ( 'NONE',  ( -12.99553232110414491, 58.19864449459908684, 25.99106464220826851 ) ) ;
#12356 = EDGE_CURVE ( 'NONE', #9516, #1913, #105, .T. ) ;
#12357 = AXIS2_PLACEMENT_3D ( 'NONE', #3003, #8400, #7073 ) ;
#12358 = AXIS2_PLACEMENT_3D ( 'NONE', #5738, #2657, #3551 ) ;
#12359 = EDGE_CURVE ( 'NONE', #9880, #10854, #3430, .T. ) ;
#12360 = ORIENTED_EDGE ( 'NONE', *, *, #9620, .T. ) ;
#12361 = CARTESIAN_POINT ( 'NONE',  ( 10.69346802281034847, -25.79937747632526879, 2.619144277183853555E-15 ) ) ;
#12362 = CARTESIAN_POINT ( 'NONE',  ( 7.668969345093573864, -75.54545454545474570, 6.730503492161126644 ) ) ;
#12363 = EDGE_LOOP ( 'NONE', ( #1245, #9487, #9238, #12658 ) ) ;
#12364 = CARTESIAN_POINT ( 'NONE',  ( 8.862685984072301792, -71.63821981287377128, 4.927609687620887691 ) ) ;
#12365 = VECTOR ( 'NONE', #3437, 1000.000000000000000 ) ;
#12366 = CARTESIAN_POINT ( 'NONE',  ( 6.764234067549970142, -111.2727272727265699, -0.6609924544552198133 ) ) ;
#12367 = DIRECTION ( 'NONE',  ( -0.000000000000000000, -0.000000000000000000, -1.000000000000000000 ) ) ;
#12368 = CARTESIAN_POINT ( 'NONE',  ( 2.557893175568158206, -128.7272727272670352, -3.337007314118542567 ) ) ;
#12369 = DIRECTION ( 'NONE',  ( 0.000000000000000000, 0.000000000000000000, 1.000000000000000000 ) ) ;
#12370 = EDGE_CURVE ( 'NONE', #12738, #7744, #3419, .T. ) ;
#12371 = DIRECTION ( 'NONE',  ( -0.000000000000000000, -0.000000000000000000, -1.000000000000000000 ) ) ;
#12372 = EDGE_CURVE ( 'NONE', #5632, #369, #8705, .T. ) ;
#12373 = VERTEX_POINT ( 'NONE', #175 ) ;
#12374 = ORIENTED_EDGE ( 'NONE', *, *, #10624, .F. ) ;
#12375 = VERTEX_POINT ( 'NONE', #11730 ) ;
#12376 = CARTESIAN_POINT ( 'NONE',  ( -6.999999999999999112, -35.00000000000000000, 7.500000000000000000 ) ) ;
#12377 = ORIENTED_EDGE ( 'NONE', *, *, #12082, .F. ) ;
#12378 = EDGE_CURVE ( 'NONE', #13845, #11915, #6572, .T. ) ;
#12379 = ADVANCED_FACE ( 'NONE', ( #7584 ), #13010, .T. ) ;
#12380 = VECTOR ( 'NONE', #11466, 1000.000000000000000 ) ;
#12381 = CARTESIAN_POINT ( 'NONE',  ( 6.201497802824914807, -111.6673017749467078, -0.6065233957951752242 ) ) ;
#12382 = FACE_BOUND ( 'NONE', #12763, .T. ) ;
#12383 = CYLINDRICAL_SURFACE ( 'NONE', #11091, 9.000000000008999024 ) ;
#12384 = DIRECTION ( 'NONE',  ( -0.9960067511297463483, 0.08927794634716618161, -4.818676322152979407E-17 ) ) ;
#12385 = VERTEX_POINT ( 'NONE', #6669 ) ;
#12386 = FACE_OUTER_BOUND ( 'NONE', #8117, .T. ) ;
#12387 = CARTESIAN_POINT ( 'NONE',  ( -0.9917158832135428703, -156.3625650723581941, -1.200616968270185048 ) ) ;
#12388 = CYLINDRICAL_SURFACE ( 'NONE', #10336, 15.29705854078139460 ) ;
#12389 = FACE_OUTER_BOUND ( 'NONE', #11936, .T. ) ;
#12390 = FACE_OUTER_BOUND ( 'NONE', #11156, .T. ) ;
#12391 = EDGE_CURVE ( 'NONE', #2835, #3968, #10870, .T. ) ;
#12392 = CARTESIAN_POINT ( 'NONE',  ( -19.51309799441515125, 26.83545189264576791, -4.432601239563245699 ) ) ;
#12393 = CARTESIAN_POINT ( 'NONE',  ( -10.69381717166375623, 63.25855867215299355, -1.533026014780321478E-15 ) ) ;
#12394 = ADVANCED_FACE ( 'NONE', ( #4567, #13089 ), #2262, .T. ) ;
#12395 = ORIENTED_EDGE ( 'NONE', *, *, #660, .T. ) ;
#12396 = TOROIDAL_SURFACE ( 'NONE', #8566, 71.99999999999998579, 2.000000000000000000 ) ;
#12397 = CARTESIAN_POINT ( 'NONE',  ( -1.800977217388287643, -65.63636364672284174, -1.354836293040065032 ) ) ;
#12398 = AXIS2_PLACEMENT_3D ( 'NONE', #10004, #13184, #3531 ) ;
#12399 = ORIENTED_EDGE ( 'NONE', *, *, #7567, .F. ) ;
#12400 = VERTEX_POINT ( 'NONE', #3304 ) ;
#12401 = CARTESIAN_POINT ( 'NONE',  ( -4.330127018922195425, 92.00000000000000000, -2.500000000000000000 ) ) ;
#12402 = CARTESIAN_POINT ( 'NONE',  ( -15.70039857998626864, -16.66659488452782156, 0.6827713257413515757 ) ) ;
#12403 =( BOUNDED_SURFACE ( )  B_SPLINE_SURFACE ( 3, 3, ( 
 ( #12934, #4412, #7508, #10728 ),
 ( #304, #13146, #3434, #5472 ),
 ( #12068, #11789, #12866, #2179 ),
 ( #9901, #6737, #4557, #7778 ) ),
 .UNSPECIFIED., .F., .F., .F. ) 
 B_SPLINE_SURFACE_WITH_KNOTS ( ( 4, 4 ),
 ( 4, 4 ),
 ( 0.000000000000000000, 1.000000000000000000 ),
 ( 0.000000000000000000, 1.000000000000000000 ),
 .UNSPECIFIED. ) 
 GEOMETRIC_REPRESENTATION_ITEM ( )  RATIONAL_B_SPLINE_SURFACE ( (
 ( 1.000000000000000000, 0.3333333333333334259, 0.3333333333333334259, 1.000000000000000000),
 ( 1.000000000000000000, 0.3333333333333334259, 0.3333333333333334259, 1.000000000000000000),
 ( 1.000000000000000000, 0.3333333333333334259, 0.3333333333333334259, 1.000000000000000000),
 ( 1.000000000000000000, 0.3333333333333334259, 0.3333333333333334259, 1.000000000000000000) ) ) 
 REPRESENTATION_ITEM ( '' )  SURFACE ( )  );
#12404 = CARTESIAN_POINT ( 'NONE',  ( -18.84535726877603423, -167.3636363590141229, -7.741214182183449921 ) ) ;
#12405 = CARTESIAN_POINT ( 'NONE',  ( -35.00000000000000000, -4.286263797015736496E-15, 7.500000000000000000 ) ) ;
#12406 = DIRECTION ( 'NONE',  ( -1.000000000000000000, 0.000000000000000000, 0.000000000000000000 ) ) ;
#12407 = CARTESIAN_POINT ( 'NONE',  ( 42.16244658108817589, 105.4500712252157655, 2.499999999999999556 ) ) ;
#12408 = DIRECTION ( 'NONE',  ( 0.4545454545454570283, 0.8907235428302452407, 0.000000000000000000 ) ) ;
#12409 = VERTEX_POINT ( 'NONE', #9634 ) ;
#12410 = VECTOR ( 'NONE', #11799, 1000.000000000000000 ) ;
#12411 = CARTESIAN_POINT ( 'NONE',  ( -8.634227980725805551, -88.04976197785512682, 2.978358350864825255 ) ) ;
#12412 = VERTEX_POINT ( 'NONE', #5481 ) ;
#12413 =( LENGTH_UNIT ( ) NAMED_UNIT ( * ) SI_UNIT ( .MILLI., .METRE. ) );
#12414 = DIRECTION ( 'NONE',  ( -6.158143864569485777E-17, -2.736152283717910599E-16, 1.000000000000000000 ) ) ;
#12415 = AXIS2_PLACEMENT_3D ( 'NONE', #10510, #5185, #8210 ) ;
#12416 = CYLINDRICAL_SURFACE ( 'NONE', #6500, 24.99999999999998934 ) ;
#12417 = DIRECTION ( 'NONE',  ( 0.8907235428302473501, 0.4545454545454531425, -6.308085367188369928E-15 ) ) ;
#12418 = CARTESIAN_POINT ( 'NONE',  ( -5.784531816357078249, -115.5952484847508117, 0.2985095753478224090 ) ) ;
#12419 = DIRECTION ( 'NONE',  ( 6.158143864569485777E-17, 2.736152283717910599E-16, -1.000000000000000000 ) ) ;
#12420 = ORIENTED_EDGE ( 'NONE', *, *, #6621, .F. ) ;
#12421 = ORIENTED_EDGE ( 'NONE', *, *, #9118, .F. ) ;
#12422 = ADVANCED_FACE ( 'NONE', ( #2122 ), #8778, .T. ) ;
#12423 = CARTESIAN_POINT ( 'NONE',  ( 15.29705854078138927, -27.45107625865536960, 30.59411708156278564 ) ) ;
#12424 = CARTESIAN_POINT ( 'NONE',  ( 6.374260517225430966, -76.81818181818142932, 7.989319691426051584 ) ) ;
#12425 = EDGE_LOOP ( 'NONE', ( #2500, #7349, #880, #5890 ) ) ;
#12426 = CARTESIAN_POINT ( 'NONE',  ( 3.656918997208050470, -76.68408298408331802, 9.436988895887294504 ) ) ;
#12427 =( LENGTH_UNIT ( ) NAMED_UNIT ( * ) SI_UNIT ( .MILLI., .METRE. ) );
#12428 = DIRECTION ( 'NONE',  ( 1.000000000000000000, 0.000000000000000000, 0.000000000000000000 ) ) ;
#12429 = CARTESIAN_POINT ( 'NONE',  ( 2.905947830705836399, -133.0909090908846224, -2.158723819797785826 ) ) ;
#12430 = CARTESIAN_POINT ( 'NONE',  ( 35.00000000000000000, 4.286263797015736496E-15, 4.000000000000000000 ) ) ;
#12431 = CARTESIAN_POINT ( 'NONE',  ( 15.48128881649354405, -16.40999965198128052, -2.699219240941213460 ) ) ;
#12432 = DIRECTION ( 'NONE',  ( -2.797435172181481150E-17, 1.000000000000000000, -1.765856845898762549E-18 ) ) ;
#12433 = AXIS2_PLACEMENT_3D ( 'NONE', #6066, #7173, #8230 ) ;
#12434 = ORIENTED_EDGE ( 'NONE', *, *, #13403, .T. ) ;
#12435 = ORIENTED_EDGE ( 'NONE', *, *, #1465, .T. ) ;
#12436 = ORIENTED_EDGE ( 'NONE', *, *, #1642, .T. ) ;
#12437 = CARTESIAN_POINT ( 'NONE',  ( 35.20000000000001705, 106.3999999999999915, -2.500000000000000000 ) ) ;
#12438 = CIRCLE ( 'NONE', #9739, 9.000000000008999024 ) ;
#12439 = ORIENTED_EDGE ( 'NONE', *, *, #2616, .T. ) ;
#12440 = CARTESIAN_POINT ( 'NONE',  ( 5.713079006591276432, -108.6653251258257029, -3.322691064749034862 ) ) ;
#12441 = EDGE_CURVE ( 'NONE', #4148, #11146, #5347, .T. ) ;
#12442 = CARTESIAN_POINT ( 'NONE',  ( -26.79177319725820894, -26.24642857144861807, 4.000000000000000000 ) ) ;
#12443 = CARTESIAN_POINT ( 'NONE',  ( 82.09155748149851206, -71.43674177705591433, 2.500000000000000000 ) ) ;
#12444 = ORIENTED_EDGE ( 'NONE', *, *, #12471, .F. ) ;
#12445 = CIRCLE ( 'NONE', #9748, 2.000000000000001776 ) ;
#12446 = DIRECTION ( 'NONE',  ( 0.000000000000000000, 0.000000000000000000, -1.000000000000000000 ) ) ;
#12447 = EDGE_CURVE ( 'NONE', #10453, #420, #8803, .T. ) ;
#12448 = CYLINDRICAL_SURFACE ( 'NONE', #12433, 15.29705854078138927 ) ;
#12449 = CARTESIAN_POINT ( 'NONE',  ( 39.71817523509052705, -20.60992048131556942, -2.500000000000004441 ) ) ;
#12450 = CARTESIAN_POINT ( 'NONE',  ( -0.6173387890061908800, -69.99999999999998579, 4.961742921553712549 ) ) ;
#12451 = CARTESIAN_POINT ( 'NONE',  ( 0.5292784318607320904, -80.00108554120387794, -10.03971594810948709 ) ) ;
#12452 = EDGE_CURVE ( 'NONE', #182, #11079, #10600, .T. ) ;
#12453 = DIRECTION ( 'NONE',  ( -1.000000000000000000, 0.000000000000000000, 0.000000000000000000 ) ) ;
#12454 = VECTOR ( 'NONE', #222, 1000.000000000000000 ) ;
#12455 = EDGE_CURVE ( 'NONE', #9666, #10021, #8640, .T. ) ;
#12456 = CARTESIAN_POINT ( 'NONE',  ( -15.29705854078139993, -19.91286587805129926, 3.516327053222078456E-17 ) ) ;
#12457 = CARTESIAN_POINT ( 'NONE',  ( -10.69346802281034670, -16.37459952631584059, -1.251741741247135829E-15 ) ) ;
#12458 = CARTESIAN_POINT ( 'NONE',  ( -32.50000000000000000, -3.980102097228898626E-15, 7.500000000000000000 ) ) ;
#12459 = DIRECTION ( 'NONE',  ( -2.797435172181481150E-17, 1.000000000000000000, -1.765856845898762549E-18 ) ) ;
#12460 = CIRCLE ( 'NONE', #2139, 15.29705854078139105 ) ;
#12461 = ORIENTED_EDGE ( 'NONE', *, *, #13444, .F. ) ;
#12462 = CARTESIAN_POINT ( 'NONE',  ( 10.69381717166375445, 53.83378072214353693, 1.239955467309983489E-15 ) ) ;
#12463 = CARTESIAN_POINT ( 'NONE',  ( 10.82118823930636964, -118.2727272727259731, 9.720764081409937418 ) ) ;
#12464 = AXIS2_PLACEMENT_3D ( 'NONE', #1012, #2907, #1852 ) ;
#12465 = EDGE_LOOP ( 'NONE', ( #4910, #4501, #9115, #12278, #10081, #13716, #9808, #5509, #11878, #13111, #4732, #7725 ) ) ;
#12466 = ORIENTED_EDGE ( 'NONE', *, *, #11093, .F. ) ;
#12467 = DIRECTION ( 'NONE',  ( 1.000000000000000000, 0.000000000000000000, 0.000000000000000000 ) ) ;
#12468 = CYLINDRICAL_SURFACE ( 'NONE', #4341, 2.000000000000000000 ) ;
#12469 = AXIS2_PLACEMENT_3D ( 'NONE', #11076, #12135, #12053 ) ;
#12470 = CARTESIAN_POINT ( 'NONE',  ( -8.139862572394246717E-16, 29.09759144140119957, -5.138218104596347907E-17 ) ) ;
#12471 = EDGE_CURVE ( 'NONE', #2423, #4467, #1423, .T. ) ;
#12472 = DIRECTION ( 'NONE',  ( 0.000000000000000000, 0.000000000000000000, 1.000000000000000000 ) ) ;
#12473 = CARTESIAN_POINT ( 'NONE',  ( 10.69346802281034137, 49.59884612375012836, 21.38693604562069694 ) ) ;
#12474 = PLANE ( 'NONE',  #12620 ) ;
#12475 = DIRECTION ( 'NONE',  ( -1.000000000000000000, 0.000000000000000000, 0.000000000000000000 ) ) ;
#12476 = MANIFOLD_SOLID_BREP ( 'Cut-Revolve-Thin2', #8271 ) ;
#12477 = ORIENTED_EDGE ( 'NONE', *, *, #5306, .F. ) ;
#12478 = AXIS2_PLACEMENT_3D ( 'NONE', #2992, #10428, #763 ) ;
#12479 = DIRECTION ( 'NONE',  ( -1.000000000000000000, 0.000000000000000000, 0.000000000000000000 ) ) ;
#12480 =( BOUNDED_SURFACE ( )  B_SPLINE_SURFACE ( 3, 3, ( 
 ( #1963, #12773, #10452, #853 ),
 ( #987, #12644, #5253, #6248 ),
 ( #10514, #921, #5186, #9541 ),
 ( #3143, #7555, #284, #5452 ) ),
 .UNSPECIFIED., .F., .F., .F. ) 
 B_SPLINE_SURFACE_WITH_KNOTS ( ( 4, 4 ),
 ( 4, 4 ),
 ( 0.000000000000000000, 1.000000000000000000 ),
 ( 0.000000000000000000, 1.000000000000000000 ),
 .UNSPECIFIED. ) 
 GEOMETRIC_REPRESENTATION_ITEM ( )  RATIONAL_B_SPLINE_SURFACE ( (
 ( 1.000000000000000000, 0.3333333333333334259, 0.3333333333333334259, 1.000000000000000000),
 ( 1.000000000000000000, 0.3333333333333334259, 0.3333333333333334259, 1.000000000000000000),
 ( 1.000000000000000000, 0.3333333333333334259, 0.3333333333333334259, 1.000000000000000000),
 ( 1.000000000000000000, 0.3333333333333334259, 0.3333333333333334259, 1.000000000000000000) ) ) 
 REPRESENTATION_ITEM ( '' )  SURFACE ( )  );
#12481 = EDGE_LOOP ( 'NONE', ( #2267, #11916, #3067 ) ) ;
#12482 = DIRECTION ( 'NONE',  ( 0.000000000000000000, -0.000000000000000000, 1.000000000000000000 ) ) ;
#12483 = EDGE_CURVE ( 'NONE', #12017, #8021, #3664, .T. ) ;
#12484 = AXIS2_PLACEMENT_3D ( 'NONE', #6983, #11263, #8950 ) ;
#12485 = CARTESIAN_POINT ( 'NONE',  ( 35.06230589874905945, 106.5835921350012825, 2.486789939184904874 ) ) ;
#12486 = FACE_OUTER_BOUND ( 'NONE', #2192, .T. ) ;
#12487 = CARTESIAN_POINT ( 'NONE',  ( -34.91511737228312739, 106.7798435036222742, 2.458454180825600410 ) ) ;
#12488 = CARTESIAN_POINT ( 'NONE',  ( 7.901556246067206857, -95.03441247031096850, 2.400298799947536477 ) ) ;
#12489 = DIRECTION ( 'NONE',  ( 0.000000000000000000, 1.000000000000000000, 0.000000000000000000 ) ) ;
#12490 = ORIENTED_EDGE ( 'NONE', *, *, #1987, .F. ) ;
#12491 = ORIENTED_EDGE ( 'NONE', *, *, #13534, .T. ) ;
#12492 = ORIENTED_EDGE ( 'NONE', *, *, #5940, .F. ) ;
#12493 = CARTESIAN_POINT ( 'NONE',  ( 12.99553232110414491, -7.774801155466914970, 3.182987412051232562E-15 ) ) ;
#12494 = VERTEX_POINT ( 'NONE', #11170 ) ;
#12495 = B_SPLINE_CURVE_WITH_KNOTS ( 'NONE', 3,
 ( #3402, #7681, #11962, #2354 ),
 .UNSPECIFIED., .F., .F.,
 ( 4, 4 ),
 ( 0.000000000000000000, 1.000000000000000000 ),
 .UNSPECIFIED. ) ;
#12496 = EDGE_LOOP ( 'NONE', ( #11195, #13121 ) ) ;
#12497 = DIRECTION ( 'NONE',  ( -1.000000000000000000, 0.000000000000000000, 0.000000000000000000 ) ) ;
#12498 = ORIENTED_EDGE ( 'NONE', *, *, #3817, .T. ) ;
#12499 = DIRECTION ( 'NONE',  ( 0.9960067511297463483, -0.08927794634716618161, 4.818676322152979407E-17 ) ) ;
#12500 =( NAMED_UNIT ( * ) PLANE_ANGLE_UNIT ( ) SI_UNIT ( $, .RADIAN. ) );
#12501 = CARTESIAN_POINT ( 'NONE',  ( -15.29705854078139460, 46.06057977201469100, 30.59411708156277498 ) ) ;
#12502 = CYLINDRICAL_SURFACE ( 'NONE', #7427, 25.50000000002549783 ) ;
#12503 = DIRECTION ( 'NONE',  ( -0.08715574274765883200, 0.9961946980917454342, 0.000000000000000000 ) ) ;
#12504 = CARTESIAN_POINT ( 'NONE',  ( 32.95454545454546036, 135.5876619995293026, 7.500000000000000000 ) ) ;
#12505 = CIRCLE ( 'NONE', #11370, 9.000000000008999024 ) ;
#12506 = CARTESIAN_POINT ( 'NONE',  ( -0.5318696992121811906, -153.1606381718178227, -1.636362426323313413 ) ) ;
#12507 = CARTESIAN_POINT ( 'NONE',  ( 22.00000000000000355, -34.99999999999999289, -7.500000000000000000 ) ) ;
#12508 = EDGE_LOOP ( 'NONE', ( #13881, #1767, #2157, #1138, #665, #3878, #8416, #5049 ) ) ;
#12509 = ORIENTED_EDGE ( 'NONE', *, *, #101, .T. ) ;
#12510 = EDGE_CURVE ( 'NONE', #8361, #7055, #13342, .T. ) ;
#12511 = ORIENTED_EDGE ( 'NONE', *, *, #12722, .F. ) ;
#12512 = ORIENTED_EDGE ( 'NONE', *, *, #10136, .F. ) ;
#12513 = CARTESIAN_POINT ( 'NONE',  ( 3.062175308430663989, -118.9477956384829582, 4.375409443047287184 ) ) ;
#12514 = AXIS2_PLACEMENT_3D ( 'NONE', #1393, #363, #12922 ) ;
#12515 = CARTESIAN_POINT ( 'NONE',  ( -8.139862572394246717E-16, 29.09759144140119957, -5.138218104596347907E-17 ) ) ;
#12516 = CARTESIAN_POINT ( 'NONE',  ( 25.00000000000000355, 120.0000000000000284, -0.5000000000000000000 ) ) ;
#12517 = DIRECTION ( 'NONE',  ( -0.000000000000000000, -0.000000000000000000, -1.000000000000000000 ) ) ;
#12518 = CARTESIAN_POINT ( 'NONE',  ( -1.853002570266264915, -151.7308256017814188, 0.1000873228714606461 ) ) ;
#12519 = DIRECTION ( 'NONE',  ( -0.7999999999999999334, -0.6000000000000001998, 0.000000000000000000 ) ) ;
#12520 = CARTESIAN_POINT ( 'NONE',  ( 0.09220535803714466350, -163.8787878952597907, -3.538661136606733315 ) ) ;
#12521 = DIRECTION ( 'NONE',  ( 1.000000000000000000, 0.000000000000000000, 0.000000000000000000 ) ) ;
#12522 = DIRECTION ( 'NONE',  ( 0.8907235428302473501, -0.4545454545454531425, 0.000000000000000000 ) ) ;
#12523 = DIRECTION ( 'NONE',  ( 0.9960067511297463483, -0.08927794634716618161, 4.818676322152979407E-17 ) ) ;
#12524 = AXIS2_PLACEMENT_3D ( 'NONE', #1470, #7850, #2524 ) ;
#12525 = CYLINDRICAL_SURFACE ( 'NONE', #9647, 15.29705854078139105 ) ;
#12526 = DIRECTION ( 'NONE',  ( 0.000000000000000000, 0.000000000000000000, 1.000000000000000000 ) ) ;
#12527 = VECTOR ( 'NONE', #1413, 1000.000000000000000 ) ;
#12528 = EDGE_CURVE ( 'NONE', #9083, #9012, #4842, .T. ) ;
#12529 = ADVANCED_FACE ( 'NONE', ( #12230 ), #658, .T. ) ;
#12530 = CARTESIAN_POINT ( 'NONE',  ( -8.827136188495221389E-16, 31.55439052270045508, -5.572053652267360357E-17 ) ) ;
#12531 = EDGE_LOOP ( 'NONE', ( #10463, #10451, #6705, #5219 ) ) ;
#12532 = CARTESIAN_POINT ( 'NONE',  ( 42.16244658108818300, 105.4500712252157655, -2.499999999999998668 ) ) ;
#12533 = EDGE_LOOP ( 'NONE', ( #5366, #12057 ) ) ;
#12534 = CARTESIAN_POINT ( 'NONE',  ( -12.09338464843077077, -61.00000000000002842, 0.006909782851250131745 ) ) ;
#12535 = EDGE_CURVE ( 'NONE', #2174, #3082, #4927, .T. ) ;
#12536 = EDGE_CURVE ( 'NONE', #4522, #2108, #5495, .T. ) ;
#12537 = VERTEX_POINT ( 'NONE', #9137 ) ;
#12538 = AXIS2_PLACEMENT_3D ( 'NONE', #11042, #554, #1440 ) ;
#12539 = ORIENTED_EDGE ( 'NONE', *, *, #11312, .T. ) ;
#12540 = CARTESIAN_POINT ( 'NONE',  ( 1.958204620527036497E-15, -70.00000000000000000, 1.236099792129133461E-16 ) ) ;
#12541 = CYLINDRICAL_SURFACE ( 'NONE', #8811, 25.00000000000000711 ) ;
#12542 = TOROIDAL_SURFACE ( 'NONE', #13220, 22.99999999999999289, 2.000000000000000000 ) ;
#12543 = CARTESIAN_POINT ( 'NONE',  ( 15.37190086779362908, -22.55217709030014817, -3.259922557882396710 ) ) ;
#12544 = CARTESIAN_POINT ( 'NONE',  ( 8.723672207956152391, -129.7272727272730890, -9.720751085824081983 ) ) ;
#12545 = CARTESIAN_POINT ( 'NONE',  ( 12.99553232110413248, 48.77386654458962312, 25.99106464220827917 ) ) ;
#12546 = FACE_OUTER_BOUND ( 'NONE', #8294, .T. ) ;
#12547 = EDGE_CURVE ( 'NONE', #4849, #4529, #9097, .T. ) ;
#12548 = FACE_OUTER_BOUND ( 'NONE', #5284, .T. ) ;
#12549 = EDGE_CURVE ( 'NONE', #11452, #425, #2544, .T. ) ;
#12550 = CIRCLE ( 'NONE', #461, 15.29705854078139105 ) ;
#12551 = ORIENTED_EDGE ( 'NONE', *, *, #8748, .T. ) ;
#12552 = EDGE_CURVE ( 'NONE', #1069, #13048, #4157, .T. ) ;
#12553 = ADVANCED_FACE ( 'NONE', ( #8929 ), #13232, .T. ) ;
#12554 = CARTESIAN_POINT ( 'NONE',  ( -4.302448071771068250, -82.51104542591967572, 8.727548302715668171 ) ) ;
#12555 = CIRCLE ( 'NONE', #7161, 2.500000000000002220 ) ;
#12556 = ORIENTED_EDGE ( 'NONE', *, *, #4267, .T. ) ;
#12557 = VERTEX_POINT ( 'NONE', #1489 ) ;
#12558 = CARTESIAN_POINT ( 'NONE',  ( 8.385254915620294014, -22.36966495935058319, -16.77050983124058092 ) ) ;
#12559 = DIRECTION ( 'NONE',  ( -0.000000000000000000, -0.000000000000000000, -1.000000000000000000 ) ) ;
#12560 = CIRCLE ( 'NONE', #5392, 16.99999999999998934 ) ;
#12561 = AXIS2_PLACEMENT_3D ( 'NONE', #402, #13096, #11942 ) ;
#12562 = CARTESIAN_POINT ( 'NONE',  ( -8.385254915620294014, 31.55439052270045508, -16.77050983124059158 ) ) ;
#12563 = CYLINDRICAL_SURFACE ( 'NONE', #12111, 9.000000000008999024 ) ;
#12564 = CARTESIAN_POINT ( 'NONE',  ( 2.249530157828166566, -133.0425321159758880, -2.931855161479524075 ) ) ;
#12565 = ADVANCED_FACE ( 'NONE', ( #457 ), #11989, .T. ) ;
#12566 = CARTESIAN_POINT ( 'NONE',  ( 10.00024727050385920, -5.026167870790865244, -2.500000000000001776 ) ) ;
#12567 = VECTOR ( 'NONE', #8061, 1000.000000000000000 ) ;
#12568 = EDGE_LOOP ( 'NONE', ( #7014, #8351, #338, #7975 ) ) ;
#12569 = ADVANCED_FACE ( 'NONE', ( #531 ), #6960, .T. ) ;
#12570 = AXIS2_PLACEMENT_3D ( 'NONE', #8949, #13255, #6006 ) ;
#12571 = AXIS2_PLACEMENT_3D ( 'NONE', #3594, #8712, #7591 ) ;
#12572 = ORIENTED_EDGE ( 'NONE', *, *, #2669, .T. ) ;
#12573 = CARTESIAN_POINT ( 'NONE',  ( -4.330127018922195425, 91.83037361138187293, -2.499999999999999556 ) ) ;
#12574 = ORIENTED_EDGE ( 'NONE', *, *, #8666, .F. ) ;
#12575 = DIRECTION ( 'NONE',  ( 1.000000000000000000, 0.000000000000000000, 0.000000000000000000 ) ) ;
#12576 = ORIENTED_EDGE ( 'NONE', *, *, #309, .T. ) ;
#12577 = CARTESIAN_POINT ( 'NONE',  ( 9.736331930512850619, -69.99978782402618549, 2.722951059031191612 ) ) ;
#12578 = TOROIDAL_SURFACE ( 'NONE', #13725, 17.49999999999999289, 5.000000000000000000 ) ;
#12579 = CARTESIAN_POINT ( 'NONE',  ( -9.849578953073196530, -91.60173160172604412, 1.758148290372610223 ) ) ;
#12580 = CARTESIAN_POINT ( 'NONE',  ( 5.042740091284176371E-16, -18.02629830864596627, 3.183186227453577089E-17 ) ) ;
#12581 = DIRECTION ( 'NONE',  ( -0.5952233065713573579, -0.8035603370713738647, 0.000000000000000000 ) ) ;
#12582 = CIRCLE ( 'NONE', #4493, 9.000000000008999024 ) ;
#12583 = DIRECTION ( 'NONE',  ( 0.000000000000000000, 0.000000000000000000, 1.000000000000000000 ) ) ;
#12584 = VECTOR ( 'NONE', #4932, 1000.000000000000000 ) ;
#12585 = CARTESIAN_POINT ( 'NONE',  ( -2.914768773580740380, -136.4521213004123865, 1.564187473038843423 ) ) ;
#12586 = DIRECTION ( 'NONE',  ( -6.158143864569485777E-17, -2.736152283717910599E-16, 1.000000000000000000 ) ) ;
#12587 = ORIENTED_EDGE ( 'NONE', *, *, #11158, .F. ) ;
#12588 = EDGE_LOOP ( 'NONE', ( #13552, #3077, #10334, #12089 ) ) ;
#12589 = VERTEX_POINT ( 'NONE', #10188 ) ;
#12590 = CIRCLE ( 'NONE', #6308, 2.000000000000001776 ) ;
#12591 = CARTESIAN_POINT ( 'NONE',  ( -15.29705854078138749, 38.52236939141059935, -2.009399357253887220E-15 ) ) ;
#12592 = ORIENTED_EDGE ( 'NONE', *, *, #5771, .T. ) ;
#12593 = CARTESIAN_POINT ( 'NONE',  ( 34.99999999999999289, 25.00000000000002132, 7.500000000000000000 ) ) ;
#12594 = CARTESIAN_POINT ( 'NONE',  ( 6.068924878052031069, -84.14159528350513995, -7.406228478373899193 ) ) ;
#12595 = FACE_OUTER_BOUND ( 'NONE', #10153, .T. ) ;
#12596 = DIRECTION ( 'NONE',  ( 0.000000000000000000, 0.000000000000000000, 1.000000000000000000 ) ) ;
#12597 = CARTESIAN_POINT ( 'NONE',  ( 0.000000000000000000, 71.01020514433645303, -0.5000000000000000000 ) ) ;
#12598 = CARTESIAN_POINT ( 'NONE',  ( 43.29712336220986657, 19.44704974301885159, 2.500000000000005773 ) ) ;
#12599 = CARTESIAN_POINT ( 'NONE',  ( 7.000000000000007994, -35.00000000000000000, -7.500000000000000000 ) ) ;
#12600 = DIRECTION ( 'NONE',  ( 1.000000000000000000, 1.665334536937735599E-15, 0.000000000000000000 ) ) ;
#12601 = CIRCLE ( 'NONE', #280, 25.00000000000000355 ) ;
#12602 = B_SPLINE_CURVE_WITH_KNOTS ( 'NONE', 3,
 ( #8605, #5374, #1182, #6711 ),
 .UNSPECIFIED., .F., .F.,
 ( 4, 4 ),
 ( 0.03713967652845534539, 0.04074225392669957035 ),
 .UNSPECIFIED. ) ;
#12603 = ORIENTED_EDGE ( 'NONE', *, *, #4759, .T. ) ;
#12604 = DIRECTION ( 'NONE',  ( -0.000000000000000000, -0.000000000000000000, -1.000000000000000000 ) ) ;
#12605 = CARTESIAN_POINT ( 'NONE',  ( -4.588105241658432476, -161.0909090906812082, 0.3432044964271254162 ) ) ;
#12606 = EDGE_LOOP ( 'NONE', ( #10827, #7307, #12130, #11000 ) ) ;
#12607 = DIRECTION ( 'NONE',  ( 0.000000000000000000, 0.000000000000000000, 1.000000000000000000 ) ) ;
#12608 = ORIENTED_EDGE ( 'NONE', *, *, #5147, .T. ) ;
#12609 = DIRECTION ( 'NONE',  ( 0.000000000000000000, 0.000000000000000000, 1.000000000000000000 ) ) ;
#12610 = CARTESIAN_POINT ( 'NONE',  ( -8.385254915620292238, -3.520109059331727686, 6.216008680731233110E-18 ) ) ;
#12611 = EDGE_CURVE ( 'NONE', #12961, #3769, #11099, .T. ) ;
#12612 = CARTESIAN_POINT ( 'NONE',  ( 15.04986406078724848, -22.34153611474686230, -4.519294538364309943 ) ) ;
#12613 = CONTEXT_DEPENDENT_SHAPE_REPRESENTATION ( #1016, #8891 ) ;
#12614 = ADVANCED_FACE ( 'NONE', ( #6255 ), #13731, .T. ) ;
#12615 = CARTESIAN_POINT ( 'NONE',  ( 3.867425345466886100, -111.7272727272767554, -3.383301718857324225 ) ) ;
#12616 = CARTESIAN_POINT ( 'NONE',  ( 15.29705854078139282, 74.33491362204294717, 1.740418857596141236E-15 ) ) ;
#12617 = DIRECTION ( 'NONE',  ( 0.9960067511297463483, -0.08927794634716618161, 4.818676322152979407E-17 ) ) ;
#12618 = LINE ( 'NONE', #7201, #3642 ) ;
#12619 = LINE ( 'NONE', #7268, #9161 ) ;
#12620 = AXIS2_PLACEMENT_3D ( 'NONE', #6292, #10430, #4173 ) ;
#12621 = ORIENTED_EDGE ( 'NONE', *, *, #3984, .F. ) ;
#12622 = CARTESIAN_POINT ( 'NONE',  ( -2.081238242702796892, -80.78225910474277782, 9.793491045833961905 ) ) ;
#12623 = EDGE_CURVE ( 'NONE', #5087, #1587, #5957, .T. ) ;
#12624 = CIRCLE ( 'NONE', #6563, 9.000000000008999024 ) ;
#12625 = ORIENTED_EDGE ( 'NONE', *, *, #7825, .F. ) ;
#12626 = CIRCLE ( 'NONE', #3404, 8.385254915620292238 ) ;
#12627 = CARTESIAN_POINT ( 'NONE',  ( -10.69381717166375623, -21.56444287793185666, -2.596402595788921324E-15 ) ) ;
#12628 = EDGE_CURVE ( 'NONE', #7723, #13532, #13389, .T. ) ;
#12629 = CARTESIAN_POINT ( 'NONE',  ( -35.04450421339218025, 112.5597086678580609, 7.500000000000000000 ) ) ;
#12630 = DIRECTION ( 'NONE',  ( 0.000000000000000000, 0.000000000000000000, 1.000000000000000000 ) ) ;
#12631 = EDGE_CURVE ( 'NONE', #4480, #11806, #2595, .T. ) ;
#12632 = CARTESIAN_POINT ( 'NONE',  ( -12.99553232110414136, 58.19864449459907974, -1.797034655631248355E-15 ) ) ;
#12633 = ADVANCED_FACE ( 'NONE', ( #1841 ), #4006, .F. ) ;
#12634 = CARTESIAN_POINT ( 'NONE',  ( -0.07087239851500722054, -158.6804527307045873, 1.494076624346223792 ) ) ;
#12635 = CARTESIAN_POINT ( 'NONE',  ( 15.29705854078139282, 47.94714734142005597, -30.59411708156277498 ) ) ;
#12636 = ORIENTED_EDGE ( 'NONE', *, *, #5842, .F. ) ;
#12637 = CYLINDRICAL_SURFACE ( 'NONE', #706, 9.000000000008999024 ) ;
#12638 = CARTESIAN_POINT ( 'NONE',  ( -12.99553232110414847, -7.774801155466916747, 25.99106464220827917 ) ) ;
#12639 = ORIENTED_EDGE ( 'NONE', *, *, #3442, .T. ) ;
#12640 = CARTESIAN_POINT ( 'NONE',  ( -35.00000000000000000, -4.286263797015736496E-15, 7.500000000000000000 ) ) ;
#12641 = EDGE_CURVE ( 'NONE', #13124, #1407, #3045, .T. ) ;
#12642 = ORIENTED_EDGE ( 'NONE', *, *, #1064, .T. ) ;
#12643 = VERTEX_POINT ( 'NONE', #12507 ) ;
#12644 = CARTESIAN_POINT ( 'NONE',  ( 10.69346802281035025, 77.87317997377837742, -21.38693604562069339 ) ) ;
#12645 = VERTEX_POINT ( 'NONE', #10462 ) ;
#12646 = DIRECTION ( 'NONE',  ( 0.9960067511297463483, -0.08927794634716618161, 4.818676322152979407E-17 ) ) ;
#12647 = AXIS2_PLACEMENT_3D ( 'NONE', #5623, #6474, #3240 ) ;
#12648 = CARTESIAN_POINT ( 'NONE',  ( -0.6173387890061912131, -70.00000000000000000, 4.961742921553712549 ) ) ;
#12649 = CYLINDRICAL_SURFACE ( 'NONE', #3389, 22.00000000000000000 ) ;
#12650 = DIRECTION ( 'NONE',  ( -1.601283208593975514E-16, 1.000000000000000000, -0.000000000000000000 ) ) ;
#12651 = ADVANCED_FACE ( 'NONE', ( #7361 ), #13590, .T. ) ;
#12652 = DIRECTION ( 'NONE',  ( -0.000000000000000000, -0.000000000000000000, -1.000000000000000000 ) ) ;
#12653 = CARTESIAN_POINT ( 'NONE',  ( -1.181099040078819939, -130.2509440800175469, 3.835336864914359101 ) ) ;
#12654 = ORIENTED_EDGE ( 'NONE', *, *, #11067, .F. ) ;
#12655 = ORIENTED_EDGE ( 'NONE', *, *, #3780, .T. ) ;
#12656 = EDGE_LOOP ( 'NONE', ( #3813, #8578, #3684, #2106 ) ) ;
#12657 = DIRECTION ( 'NONE',  ( 0.9960067511297464593, -0.08927794634716622324, 3.401418580343279473E-17 ) ) ;
#12658 = ORIENTED_EDGE ( 'NONE', *, *, #6436, .F. ) ;
#12659 = CARTESIAN_POINT ( 'NONE',  ( -25.00000000000000355, 120.0000000000000284, 0.5000000000000000000 ) ) ;
#12660 = CARTESIAN_POINT ( 'NONE',  ( 2.715127098185230459, -81.24690994262827815, -9.545145086786032351 ) ) ;
#12661 = VECTOR ( 'NONE', #1247, 1000.000000000000000 ) ;
#12662 = FACE_OUTER_BOUND ( 'NONE', #321, .T. ) ;
#12663 = CARTESIAN_POINT ( 'NONE',  ( 12.99579180576517246, 64.08350967699263379, -25.99158361153033425 ) ) ;
#12664 = CIRCLE ( 'NONE', #11742, 66.25000000000044054 ) ;
#12665 = CYLINDRICAL_SURFACE ( 'NONE', #1568, 2.500000000000000444 ) ;
#12666 = CARTESIAN_POINT ( 'NONE',  ( -25.00000000000000355, 120.0000000000000142, 0.5000000000000000000 ) ) ;
#12667 = DIRECTION ( 'NONE',  ( -1.000000000000000000, 0.000000000000000000, 0.000000000000000000 ) ) ;
#12668 = AXIS2_PLACEMENT_3D ( 'NONE', #742, #12517, #5007 ) ;
#12669 = CYLINDRICAL_SURFACE ( 'NONE', #5920, 8.385254915620292238 ) ;
#12670 = DIRECTION ( 'NONE',  ( 0.000000000000000000, 0.000000000000000000, 1.000000000000000000 ) ) ;
#12671 = ORIENTED_EDGE ( 'NONE', *, *, #1463, .T. ) ;
#12672 = LINE ( 'NONE', #11603, #6712 ) ;
#12673 = AXIS2_PLACEMENT_3D ( 'NONE', #3435, #5537, #10730 ) ;
#12674 = ORIENTED_EDGE ( 'NONE', *, *, #9583, .F. ) ;
#12675 = CARTESIAN_POINT ( 'NONE',  ( 10.69381717166375267, -12.13966492792242846, 21.38763434332751601 ) ) ;
#12676 = ORIENTED_EDGE ( 'NONE', *, *, #4296, .T. ) ;
#12677 = DIRECTION ( 'NONE',  ( 1.000000000000000000, -0.000000000000000000, -0.000000000000000000 ) ) ;
#12678 = FACE_OUTER_BOUND ( 'NONE', #1400, .T. ) ;
#12679 = CARTESIAN_POINT ( 'NONE',  ( 32.61455173758670867, 25.38817907193537593, 7.372574772901430151E-15 ) ) ;
#12680 = CARTESIAN_POINT ( 'NONE',  ( 11.42522452384381459, -72.18181818184932297, 3.860454353695761842 ) ) ;
#12681 = DIRECTION ( 'NONE',  ( 1.000000000000000000, 6.530723674265631117E-15, 0.000000000000000000 ) ) ;
#12682 = CARTESIAN_POINT ( 'NONE',  ( -8.385254915620292238, -22.36966495935058319, 16.77050983124057737 ) ) ;
#12683 = VECTOR ( 'NONE', #6818, 1000.000000000000000 ) ;
#12684 = DIRECTION ( 'NONE',  ( -1.000000000000000000, 0.000000000000000000, 0.000000000000000000 ) ) ;
#12685 = CARTESIAN_POINT ( 'NONE',  ( -4.696430422119474812, 90.40949893945196436, 1.719416569030751907 ) ) ;
#12686 = ADVANCED_FACE ( 'NONE', ( #1975 ), #11646, .F. ) ;
#12687 = ORIENTED_EDGE ( 'NONE', *, *, #11261, .T. ) ;
#12688 = CARTESIAN_POINT ( 'NONE',  ( -2.712777076799875786, -81.24515448198224021, 9.546134740491345028 ) ) ;
#12689 = AXIS2_PLACEMENT_3D ( 'NONE', #2872, #8133, #7146 ) ;
#12690 = ORIENTED_EDGE ( 'NONE', *, *, #12735, .T. ) ;
#12691 = CARTESIAN_POINT ( 'NONE',  ( 12.99579180576517246, -11.31471392308272428, -25.99158361153033070 ) ) ;
#12692 = CARTESIAN_POINT ( 'NONE',  ( 10.00000000000000711, 139.9999999999999716, -0.5000000000000000000 ) ) ;
#12693 = DIRECTION ( 'NONE',  ( 1.000000000000000000, 0.000000000000000000, 0.000000000000000000 ) ) ;
#12694 = CARTESIAN_POINT ( 'NONE',  ( 25.00000000000000355, 120.0000000000000142, -0.5000000000000000000 ) ) ;
#12695 = DIRECTION ( 'NONE',  ( 1.000000000000000000, 0.000000000000000000, 0.000000000000000000 ) ) ;
#12696 = CARTESIAN_POINT ( 'NONE',  ( -15.18222645069203303, -16.04698886238941924, -4.000000000000000000 ) ) ;
#12697 = EDGE_CURVE ( 'NONE', #2174, #13136, #11763, .T. ) ;
#12698 = ORIENTED_EDGE ( 'NONE', *, *, #1082, .F. ) ;
#12699 = EDGE_CURVE ( 'NONE', #12324, #6913, #8358, .T. ) ;
#12700 = VERTEX_POINT ( 'NONE', #2823 ) ;
#12701 = EDGE_CURVE ( 'NONE', #9446, #12162, #6850, .T. ) ;
#12702 = DIRECTION ( 'NONE',  ( -0.5999999999999982014, -0.8000000000000013767, -0.000000000000000000 ) ) ;
#12703 = ADVANCED_FACE ( 'NONE', ( #5126 ), #10433, .T. ) ;
#12704 = EDGE_CURVE ( 'NONE', #11706, #10135, #13820, .T. ) ;
#12705 = ORIENTED_EDGE ( 'NONE', *, *, #1118, .F. ) ;
#12706 = CARTESIAN_POINT ( 'NONE',  ( -3.163850051431345456, 90.09728930184206774, -3.875191615614280494 ) ) ;
#12707 = AXIS2_PLACEMENT_3D ( 'NONE', #11749, #4439, #3391 ) ;
#12708 = CARTESIAN_POINT ( 'NONE',  ( 35.00000000000001421, -34.99999999999999289, -4.000000000000000000 ) ) ;
#12709 = ORIENTED_EDGE ( 'NONE', *, *, #11312, .F. ) ;
#12710 = CARTESIAN_POINT ( 'NONE',  ( 0.9875500501441598633, -80.00464164738322381, -10.06307372056550342 ) ) ;
#12711 = PLANE ( 'NONE',  #5791 ) ;
#12712 = CARTESIAN_POINT ( 'NONE',  ( -9.883290025451492156, -71.99999999999975842, -4.866269441041104926 ) ) ;
#12713 = CYLINDRICAL_SURFACE ( 'NONE', #11556, 18.74900000001875000 ) ;
#12714 = LINE ( 'NONE', #2841, #9927 ) ;
#12715 = CARTESIAN_POINT ( 'NONE',  ( -0.5859240664712906943, -103.8004541631269291, -7.169336856130571256 ) ) ;
#12716 = DIRECTION ( 'NONE',  ( -0.000000000000000000, -0.000000000000000000, -1.000000000000000000 ) ) ;
#12717 = ORIENTED_EDGE ( 'NONE', *, *, #1214, .F. ) ;
#12718 = VERTEX_POINT ( 'NONE', #1765 ) ;
#12719 = CARTESIAN_POINT ( 'NONE',  ( 62.16766351966359849, -73.17985663200910551, 2.500000000000000000 ) ) ;
#12720 = ORIENTED_EDGE ( 'NONE', *, *, #6436, .T. ) ;
#12721 = DIRECTION ( 'NONE',  ( -1.000000000000000000, 0.000000000000000000, 0.000000000000000000 ) ) ;
#12722 = EDGE_CURVE ( 'NONE', #11569, #12930, #7721, .T. ) ;
#12723 = CARTESIAN_POINT ( 'NONE',  ( 12.99553232110413781, 39.34908859458022334, 3.182987412051230984E-15 ) ) ;
#12724 = CARTESIAN_POINT ( 'NONE',  ( 25.00000000000000355, 120.0000000000000142, -2.499999999999998668 ) ) ;
#12725 = CARTESIAN_POINT ( 'NONE',  ( -6.124978294105043908, -112.7307712075077006, -0.3410559919339725132 ) ) ;
#12726 = DIRECTION ( 'NONE',  ( -0.000000000000000000, -0.000000000000000000, -1.000000000000000000 ) ) ;
#12727 = DIRECTION ( 'NONE',  ( -1.000000000000000000, 0.000000000000000000, 0.000000000000000000 ) ) ;
#12728 = FACE_OUTER_BOUND ( 'NONE', #9606, .T. ) ;
#12729 = CARTESIAN_POINT ( 'NONE',  ( -15.29705854078138927, 0.8232575913729157646, -30.59411708156278564 ) ) ;
#12730 = CARTESIAN_POINT ( 'NONE',  ( 35.20000000000002416, 106.4000000000000199, 0.5000000000000000000 ) ) ;
#12731 = CYLINDRICAL_SURFACE ( 'NONE', #4113, 25.50000000002550138 ) ;
#12732 = DIRECTION ( 'NONE',  ( -2.797435172181481150E-17, 1.000000000000000000, -1.765856845898762549E-18 ) ) ;
#12733 = DIRECTION ( 'NONE',  ( 1.000000000000000000, 0.000000000000000000, 0.000000000000000000 ) ) ;
#12734 = CARTESIAN_POINT ( 'NONE',  ( -11.42522452383575526, -72.18181818187404986, -3.860454353694361629 ) ) ;
#12735 = EDGE_CURVE ( 'NONE', #3156, #7206, #10330, .T. ) ;
#12736 = EDGE_LOOP ( 'NONE', ( #9725, #7459, #2024, #1343, #1962, #5811 ) ) ;
#12737 = FACE_OUTER_BOUND ( 'NONE', #10909, .T. ) ;
#12738 = VERTEX_POINT ( 'NONE', #13658 ) ;
#12739 = CARTESIAN_POINT ( 'NONE',  ( 15.29705854078139105, -10.48808792804187284, 1.890204135573039875E-15 ) ) ;
#12740 = CARTESIAN_POINT ( 'NONE',  ( -25.00000000000000355, 120.0000000000000284, -2.500000000000000000 ) ) ;
#12741 = FACE_OUTER_BOUND ( 'NONE', #13523, .T. ) ;
#12742 = CARTESIAN_POINT ( 'NONE',  ( -5.138450363093652662, -111.7272727272696642, 0.006098328147121623993 ) ) ;
#12743 = CIRCLE ( 'NONE', #1529, 15.29705854078139105 ) ;
#12744 = LINE ( 'NONE', #9453, #7174 ) ;
#12745 = DIRECTION ( 'NONE',  ( 1.000000000000000000, 0.000000000000000000, 0.000000000000000000 ) ) ;
#12746 = CARTESIAN_POINT ( 'NONE',  ( 2.933974605883639275E-16, -10.48808792804187284, 1.852046186812095429E-17 ) ) ;
#12747 = DIRECTION ( 'NONE',  ( -1.000000000000000000, 0.000000000000000000, 0.000000000000000000 ) ) ;
#12748 = CARTESIAN_POINT ( 'NONE',  ( 30.29366116764611760, 20.61262658154624816, -2.499999999999993783 ) ) ;
#12749 = CIRCLE ( 'NONE', #6687, 8.385254915620292238 ) ;
#12750 = ORIENTED_EDGE ( 'NONE', *, *, #2581, .F. ) ;
#12751 = CARTESIAN_POINT ( 'NONE',  ( 0.000000000000000000, 0.000000000000000000, 0.000000000000000000 ) ) ;
#12752 = ORIENTED_EDGE ( 'NONE', *, *, #9256, .T. ) ;
#12753 = CARTESIAN_POINT ( 'NONE',  ( 8.385254915620290461, 43.60378069071538221, 9.813990265092201964E-16 ) ) ;
#12754 = CARTESIAN_POINT ( 'NONE',  ( -8.385254915620297567, 69.25350232273815720, 16.77050983124058448 ) ) ;
#12755 = EDGE_CURVE ( 'NONE', #4358, #11837, #7289, .T. ) ;
#12756 = AXIS2_PLACEMENT_3D ( 'NONE', #6396, #13666, #868 ) ;
#12757 = DIRECTION ( 'NONE',  ( 1.000000000000000000, 0.000000000000000000, 0.000000000000000000 ) ) ;
#12758 = FILL_AREA_STYLE ('',( #411 ) ) ;
#12759 = CARTESIAN_POINT ( 'NONE',  ( -8.827136188495221389E-16, 31.55439052270045508, -5.572053652267360357E-17 ) ) ;
#12760 = CIRCLE ( 'NONE', #11199, 25.50418395392908977 ) ;
#12761 =( NAMED_UNIT ( * ) PLANE_ANGLE_UNIT ( ) SI_UNIT ( $, .RADIAN. ) );
#12762 = DIRECTION ( 'NONE',  ( 1.000000000000000000, 0.000000000000000000, 0.000000000000000000 ) ) ;
#12763 = EDGE_LOOP ( 'NONE', ( #1140, #10095 ) ) ;
#12764 = ORIENTED_EDGE ( 'NONE', *, *, #8799, .T. ) ;
#12765 = EDGE_LOOP ( 'NONE', ( #5115, #8650, #9054, #9250 ) ) ;
#12766 = DIRECTION ( 'NONE',  ( 0.000000000000000000, 0.000000000000000000, 1.000000000000000000 ) ) ;
#12767 = AXIS2_PLACEMENT_3D ( 'NONE', #2906, #1988, #10471 ) ;
#12768 = AXIS2_PLACEMENT_3D ( 'NONE', #5647, #9930, #7897 ) ;
#12769 = CARTESIAN_POINT ( 'NONE',  ( -3.828914887500469266, 90.45818551217382719, -3.218881588266133686 ) ) ;
#12770 = AXIS2_PLACEMENT_3D ( 'NONE', #12532, #2064, #6276 ) ;
#12771 = ORIENTED_EDGE ( 'NONE', *, *, #11919, .F. ) ;
#12772 = ORIENTED_EDGE ( 'NONE', *, *, #1503, .T. ) ;
#12773 = CARTESIAN_POINT ( 'NONE',  ( 8.385254915620295790, 78.67828027274755698, -16.77050983124058803 ) ) ;
#12774 = ORIENTED_EDGE ( 'NONE', *, *, #13181, .T. ) ;
#12775 = DIRECTION ( 'NONE',  ( -0.7999999999999999334, -0.6000000000000001998, 0.000000000000000000 ) ) ;
#12776 = ADVANCED_FACE ( 'NONE', ( #2241, #2305 ), #6526, .T. ) ;
#12777 = DIRECTION ( 'NONE',  ( -6.158143864569485777E-17, -2.736152283717910599E-16, 1.000000000000000000 ) ) ;
#12778 = EDGE_CURVE ( 'NONE', #8282, #10214, #3466, .T. ) ;
#12779 = CARTESIAN_POINT ( 'NONE',  ( 39.06230589874904524, 109.5835921350012683, 2.499999999999999556 ) ) ;
#12780 = CARTESIAN_POINT ( 'NONE',  ( -24.99999999999999289, -99.43893449056518818, 2.967955073073089700 ) ) ;
#12781 = CARTESIAN_POINT ( 'NONE',  ( -10.69346802281034847, 68.44840202376897764, -2.779593060601867454E-15 ) ) ;
#12782 = VECTOR ( 'NONE', #8285, 1000.000000000000000 ) ;
#12783 = CARTESIAN_POINT ( 'NONE',  ( -2.891665148108589545, -140.3705018960054929, 0.05415431998640414524 ) ) ;
#12784 = CARTESIAN_POINT ( 'NONE',  ( 13.76342357120274862, 14.11587126553561689, 2.500000000000002665 ) ) ;
#12785 = ORIENTED_EDGE ( 'NONE', *, *, #10493, .F. ) ;
#12786 = AXIS2_PLACEMENT_3D ( 'NONE', #8388, #4171, #12681 ) ;
#12787 = AXIS2_PLACEMENT_3D ( 'NONE', #10726, #6535, #12066 ) ;
#12788 = VERTEX_POINT ( 'NONE', #82 ) ;
#12789 = CARTESIAN_POINT ( 'NONE',  ( 10.11726280447958182, 5.576682675210008711, 2.500000000000000000 ) ) ;
#12790 = ORIENTED_EDGE ( 'NONE', *, *, #3184, .T. ) ;
#12791 = CARTESIAN_POINT ( 'NONE',  ( 1.616533774874506480E-14, -132.0000000000000000, 0.000000000000000000 ) ) ;
#12792 = AXIS2_PLACEMENT_3D ( 'NONE', #11599, #3106, #3174 ) ;
#12793 = CARTESIAN_POINT ( 'NONE',  ( -12.99553232110412893, 39.34908859458022334, -25.99106464220826851 ) ) ;
#12794 = CARTESIAN_POINT ( 'NONE',  ( 8.641831928493635573, -88.07519045024412208, -2.946015976100306855 ) ) ;
#12795 = CIRCLE ( 'NONE', #7852, 31.93204061526060755 ) ;
#12796 = EDGE_CURVE ( 'NONE', #1178, #5471, #2371, .T. ) ;
#12797 = CARTESIAN_POINT ( 'NONE',  ( -10.69381717166375090, 6.709890972096425266, -21.38763434332751245 ) ) ;
#12798 = B_SPLINE_CURVE_WITH_KNOTS ( 'NONE', 3,
 ( #5525, #78, #3420, #10847, #4271, #1260, #6450, #6521, #10714, #13064, #9812, #4332, #8615, #7560, #10779, #1194, #4474, #5676, #5897, #9119, #641, #3783, #12274, #8978, #11288, #3634, #12350, #13209 ),
 .UNSPECIFIED., .F., .F.,
 ( 4, 2, 2, 2, 2, 2, 2, 2, 2, 2, 2, 2, 2, 4 ),
 ( 1.917168677021176670E-17, 0.002162634761238544073, 0.003243952141857817627, 0.004325269522477092482, 0.006487904283715641325, 0.008650539044954190168, 0.009731856425573476299, 0.01081317380619276416, 0.01189449118681205030, 0.01297580856743134163, 0.01513844332866991910, 0.01621976070928919655, 0.01676041939959882487, 0.01730107808990844973 ),
 .UNSPECIFIED. ) ;
#12799 = AXIS2_PLACEMENT_3D ( 'NONE', #5491, #115, #4367 ) ;
#12800 = DIRECTION ( 'NONE',  ( -1.000000000000000000, -2.835060530349835421E-17, 0.000000000000000000 ) ) ;
#12801 = ADVANCED_FACE ( 'NONE', ( #1198 ), #160, .T. ) ;
#12802 = CARTESIAN_POINT ( 'NONE',  ( -1.623329383841033646, -80.00119987276727329, -9.930725418093544477 ) ) ;
#12803 = CARTESIAN_POINT ( 'NONE',  ( -1.673669778670227307E-15, 59.82872437272870769, -1.056489625149731375E-16 ) ) ;
#12804 = DIRECTION ( 'NONE',  ( -2.797435172181481150E-17, 1.000000000000000000, -1.765856845898762549E-18 ) ) ;
#12805 = CARTESIAN_POINT ( 'NONE',  ( -42.16244658108818300, 105.4500712252157655, 2.499999999999999556 ) ) ;
#12806 = ADVANCED_FACE ( 'NONE', ( #5461 ), #9747, .T. ) ;
#12807 = CARTESIAN_POINT ( 'NONE',  ( 76.84607712649204814, -99.92541302764922762, 2.500000000000000000 ) ) ;
#12808 = EDGE_CURVE ( 'NONE', #1913, #10090, #2813, .T. ) ;
#12809 = AXIS2_PLACEMENT_3D ( 'NONE', #13875, #10542, #8506 ) ;
#12810 = VERTEX_POINT ( 'NONE', #7702 ) ;
#12811 = VECTOR ( 'NONE', #6871, 1000.000000000000000 ) ;
#12812 = CIRCLE ( 'NONE', #715, 5.000000000000000000 ) ;
#12813 = CARTESIAN_POINT ( 'NONE',  ( -10.69381717166375623, 72.68333662216238622, -2.782997899970468246E-15 ) ) ;
#12814 = ORIENTED_EDGE ( 'NONE', *, *, #11823, .T. ) ;
#12815 = CARTESIAN_POINT ( 'NONE',  ( 6.296481028488151388, -65.63636363857402500, 1.027962039518596882 ) ) ;
#12816 = VERTEX_POINT ( 'NONE', #12989 ) ;
#12817 = DIRECTION ( 'NONE',  ( 6.158143864569485777E-17, 2.736152283717910599E-16, -1.000000000000000000 ) ) ;
#12818 = ORIENTED_EDGE ( 'NONE', *, *, #3795, .F. ) ;
#12819 = DIRECTION ( 'NONE',  ( 1.000000000000000000, 0.000000000000000000, 0.000000000000000000 ) ) ;
#12820 = DIRECTION ( 'NONE',  ( -1.000000000000000000, 0.000000000000000000, 0.000000000000000000 ) ) ;
#12821 = CARTESIAN_POINT ( 'NONE',  ( -1.553027081867818682, -81.93939393924890169, 9.741774319753540468 ) ) ;
#12822 = EDGE_CURVE ( 'NONE', #11499, #10921, #11441, .T. ) ;
#12823 = LINE ( 'NONE', #8387, #2317 ) ;
#12824 = CIRCLE ( 'NONE', #44, 2.000000000000000000 ) ;
#12825 = DIRECTION ( 'NONE',  ( -2.797435172181481150E-17, 1.000000000000000000, -1.765856845898762549E-18 ) ) ;
#12826 = CARTESIAN_POINT ( 'NONE',  ( 12.99553232110413958, 11.07475474455194053, 1.577534959232427603E-15 ) ) ;
#12827 = CARTESIAN_POINT ( 'NONE',  ( -32.50000000000000000, -3.980102097228898626E-15, 7.500000000000000000 ) ) ;
#12828 = EDGE_CURVE ( 'NONE', #11308, #4855, #7565, .T. ) ;
#12829 = DIRECTION ( 'NONE',  ( 0.9960067511297464593, -0.08927794634716622324, 6.802837160686558945E-17 ) ) ;
#12830 = DIRECTION ( 'NONE',  ( 0.9960067511297463483, -0.08927794634716618161, 4.818676322152979407E-17 ) ) ;
#12831 = ORIENTED_EDGE ( 'NONE', *, *, #114, .F. ) ;
#12832 =( BOUNDED_SURFACE ( )  B_SPLINE_SURFACE ( 3, 3, ( 
 ( #6104, #2869, #12562, #4182 ),
 ( #11693, #6235, #8268, #1047 ),
 ( #10441, #1815, #2086, #8203 ),
 ( #2020, #5241, #10637, #6367 ) ),
 .UNSPECIFIED., .F., .F., .F. ) 
 B_SPLINE_SURFACE_WITH_KNOTS ( ( 4, 4 ),
 ( 4, 4 ),
 ( 0.000000000000000000, 1.000000000000000000 ),
 ( 0.000000000000000000, 1.000000000000000000 ),
 .UNSPECIFIED. ) 
 GEOMETRIC_REPRESENTATION_ITEM ( )  RATIONAL_B_SPLINE_SURFACE ( (
 ( 1.000000000000000000, 0.3333333333333334259, 0.3333333333333334259, 1.000000000000000000),
 ( 1.000000000000000000, 0.3333333333333334259, 0.3333333333333334259, 1.000000000000000000),
 ( 1.000000000000000000, 0.3333333333333334259, 0.3333333333333334259, 1.000000000000000000),
 ( 1.000000000000000000, 0.3333333333333334259, 0.3333333333333334259, 1.000000000000000000) ) ) 
 REPRESENTATION_ITEM ( '' )  SURFACE ( )  );
#12833 = CIRCLE ( 'NONE', #7203, 40.00000000000001421 ) ;
#12834 = PRESENTATION_STYLE_ASSIGNMENT (( #972 ) ) ;
#12835 = ORIENTED_EDGE ( 'NONE', *, *, #7624, .T. ) ;
#12836 = CARTESIAN_POINT ( 'NONE',  ( 25.00000000000000355, 120.0000000000000142, 2.499999999999999556 ) ) ;
#12837 = CARTESIAN_POINT ( 'NONE',  ( -35.20000000000000995, 106.3999999999999915, -0.5000000000000000000 ) ) ;
#12838 = DIRECTION ( 'NONE',  ( 0.000000000000000000, 0.000000000000000000, 1.000000000000000000 ) ) ;
#12839 = CARTESIAN_POINT ( 'NONE',  ( -3.989522564198866306, -78.56682798443820559, -9.305603802367686583 ) ) ;
#12840 = CARTESIAN_POINT ( 'NONE',  ( 0.5328336654596128596, -153.1537951631405576, 1.636456857774888807 ) ) ;
#12841 = FACE_OUTER_BOUND ( 'NONE', #12765, .T. ) ;
#12842 = ORIENTED_EDGE ( 'NONE', *, *, #12991, .F. ) ;
#12843 = ORIENTED_EDGE ( 'NONE', *, *, #6340, .T. ) ;
#12844 = CIRCLE ( 'NONE', #6784, 18.74900000001875355 ) ;
#12845 = VERTEX_POINT ( 'NONE', #8619 ) ;
#12846 = EDGE_LOOP ( 'NONE', ( #11961, #11360, #6634, #10163 ) ) ;
#12847 = LINE ( 'NONE', #5320, #2705 ) ;
#12848 = EDGE_LOOP ( 'NONE', ( #6200, #3315, #7507 ) ) ;
#12849 = CARTESIAN_POINT ( 'NONE',  ( 8.385254915620288685, 71.87811454074363837, 2.053795118489799215E-15 ) ) ;
#12850 = AXIS2_PLACEMENT_3D ( 'NONE', #7647, #10930, #11924 ) ;
#12851 = CARTESIAN_POINT ( 'NONE',  ( -27.38873514654796537, -24.33759740261776017, 4.000000000000000000 ) ) ;
#12852 =( NAMED_UNIT ( * ) PLANE_ANGLE_UNIT ( ) SI_UNIT ( $, .RADIAN. ) );
#12853 = DIRECTION ( 'NONE',  ( -0.000000000000000000, -0.000000000000000000, -1.000000000000000000 ) ) ;
#12854 = CARTESIAN_POINT ( 'NONE',  ( -12.99553232110413958, 67.62342244460847951, -3.323022390375262386E-15 ) ) ;
#12855 = VECTOR ( 'NONE', #3559, 1000.000000000000000 ) ;
#12856 = CARTESIAN_POINT ( 'NONE',  ( -3.876523907412873449, -100.4503140241744461, -6.538907747273460913 ) ) ;
#12857 = DIRECTION ( 'NONE',  ( 1.000000000000000000, 0.000000000000000000, 0.000000000000000000 ) ) ;
#12858 = VERTEX_POINT ( 'NONE', #9613 ) ;
#12859 = ORIENTED_EDGE ( 'NONE', *, *, #3984, .T. ) ;
#12860 = EDGE_LOOP ( 'NONE', ( #5349, #11299, #3935, #11715, #3844, #4369 ) ) ;
#12861 = EDGE_CURVE ( 'NONE', #6130, #5016, #1922, .T. ) ;
#12862 = AXIS2_PLACEMENT_3D ( 'NONE', #10861, #9970, #4346 ) ;
#12863 = AXIS2_PLACEMENT_3D ( 'NONE', #11121, #1508, #10068 ) ;
#12864 = DIRECTION ( 'NONE',  ( -0.000000000000000000, -0.000000000000000000, -1.000000000000000000 ) ) ;
#12865 = ORIENTED_EDGE ( 'NONE', *, *, #10557, .F. ) ;
#12866 = CARTESIAN_POINT ( 'NONE',  ( 10.69381717166375090, -2.714886977913000266, 21.38763434332751245 ) ) ;
#12867 = CYLINDRICAL_SURFACE ( 'NONE', #7972, 27.49999999999999289 ) ;
#12868 = CARTESIAN_POINT ( 'NONE',  ( -6.244934989200983111, -111.0871311010834006, 1.123163629316296541 ) ) ;
#12869 = LINE ( 'NONE', #1211, #7817 ) ;
#12870 = CARTESIAN_POINT ( 'NONE',  ( -2.739930038171048743, -137.4545454545128678, -2.373837707219439874 ) ) ;
#12871 = DIRECTION ( 'NONE',  ( 0.000000000000000000, 0.000000000000000000, -1.000000000000000000 ) ) ;
#12872 = DIRECTION ( 'NONE',  ( 0.000000000000000000, 0.000000000000000000, 1.000000000000000000 ) ) ;
#12873 = CARTESIAN_POINT ( 'NONE',  ( -9.082088619475678470, -71.90909090908878909, -4.345719731624131832 ) ) ;
#12874 = CARTESIAN_POINT ( 'NONE',  ( -35.20000000000000995, 106.4000000000000199, -2.500000000000000000 ) ) ;
#12875 = DIRECTION ( 'NONE',  ( -0.6000000000000001998, 0.7999999999999998224, -0.000000000000000000 ) ) ;
#12876 = EDGE_CURVE ( 'NONE', #9459, #9003, #9752, .T. ) ;
#12877 = CARTESIAN_POINT ( 'NONE',  ( -38.79999999999999716, 101.5999999999999943, -2.500000000000000000 ) ) ;
#12878 = DIRECTION ( 'NONE',  ( 0.9960067511297464593, -0.08927794634716622324, 3.401418580343279473E-17 ) ) ;
#12879 = ORIENTED_EDGE ( 'NONE', *, *, #2781, .F. ) ;
#12880 = ADVANCED_FACE ( 'NONE', ( #11913 ), #8194, .T. ) ;
#12881 = ORIENTED_EDGE ( 'NONE', *, *, #3548, .F. ) ;
#12882 = AXIS2_PLACEMENT_3D ( 'NONE', #4056, #11560, #3131 ) ;
#12883 = LINE ( 'NONE', #11541, #7062 ) ;
#12884 = EDGE_CURVE ( 'NONE', #1355, #1592, #1134, .T. ) ;
#12885 = ORIENTED_EDGE ( 'NONE', *, *, #10630, .F. ) ;
#12886 = AXIS2_PLACEMENT_3D ( 'NONE', #8452, #10814, #2337 ) ;
#12887 = DIRECTION ( 'NONE',  ( 0.000000000000000000, 0.000000000000000000, 1.000000000000000000 ) ) ;
#12888 = ORIENTED_EDGE ( 'NONE', *, *, #5341, .T. ) ;
#12889 = EDGE_CURVE ( 'NONE', #6792, #3113, #13068, .T. ) ;
#12890 = FACE_OUTER_BOUND ( 'NONE', #8069, .T. ) ;
#12891 = DIRECTION ( 'NONE',  ( -1.000000000000000000, 0.000000000000000000, 0.000000000000000000 ) ) ;
#12892 = AXIS2_PLACEMENT_3D ( 'NONE', #2070, #8451, #1026 ) ;
#12893 = CARTESIAN_POINT ( 'NONE',  ( -25.00000000000000355, 120.0000000000000142, 2.500000000000000000 ) ) ;
#12894 = CARTESIAN_POINT ( 'NONE',  ( 8.385254915620288685, 34.17900274070598243, 9.688596779957292534E-16 ) ) ;
#12895 = DIRECTION ( 'NONE',  ( 1.000000000000000000, 0.000000000000000000, 0.000000000000000000 ) ) ;
#12896 = CARTESIAN_POINT ( 'NONE',  ( 0.6173387890061909911, 79.99058638175036151, -4.961742921553712549 ) ) ;
#12897 = DIRECTION ( 'NONE',  ( -2.797435172181481150E-17, 1.000000000000000000, -1.765856845898762549E-18 ) ) ;
#12898 = FACE_OUTER_BOUND ( 'NONE', #9504, .T. ) ;
#12899 = AXIS2_PLACEMENT_3D ( 'NONE', #8381, #3053, #9774 ) ;
#12900 = CIRCLE ( 'NONE', #12216, 80.00000000000001421 ) ;
#12901 = EDGE_CURVE ( 'NONE', #752, #1178, #5730, .T. ) ;
#12902 = ORIENTED_EDGE ( 'NONE', *, *, #406, .T. ) ;
#12903 = CARTESIAN_POINT ( 'NONE',  ( 12.99579180576517068, 45.23395377697383424, -25.99158361153033070 ) ) ;
#12904 = TOROIDAL_SURFACE ( 'NONE', #8620, 77.99999999999997158, 2.000000000000000000 ) ;
#12905 = DIRECTION ( 'NONE',  ( -0.000000000000000000, -0.000000000000000000, -1.000000000000000000 ) ) ;
#12906 = CARTESIAN_POINT ( 'NONE',  ( 25.00000000000000711, -99.51472204732195337, 3.411167378945609840 ) ) ;
#12907 = CYLINDRICAL_SURFACE ( 'NONE', #4297, 18.74900000001875000 ) ;
#12908 = CARTESIAN_POINT ( 'NONE',  ( -25.00000000000000355, 120.0000000000000284, 0.5000000000000000000 ) ) ;
#12909 = AXIS2_PLACEMENT_3D ( 'NONE', #13792, #12716, #10524 ) ;
#12910 = CARTESIAN_POINT ( 'NONE',  ( -38.16244658108818300, 102.4500712252157797, -2.500000000000000444 ) ) ;
#12911 = DIRECTION ( 'NONE',  ( -2.797435172181481150E-17, 1.000000000000000000, -1.765856845898762549E-18 ) ) ;
#12912 = ORIENTED_EDGE ( 'NONE', *, *, #5147, .F. ) ;
#12913 = ORIENTED_EDGE ( 'NONE', *, *, #10130, .F. ) ;
#12914 = VECTOR ( 'NONE', #1839, 1000.000000000000000 ) ;
#12915 =( GEOMETRIC_REPRESENTATION_CONTEXT ( 3 ) GLOBAL_UNCERTAINTY_ASSIGNED_CONTEXT ( ( #13197 ) ) GLOBAL_UNIT_ASSIGNED_CONTEXT ( ( #9657, #11758, #4178 ) ) REPRESENTATION_CONTEXT ( 'NONE', 'WORKASPACE' ) );
#12916 = CIRCLE ( 'NONE', #3915, 15.29705854078140170 ) ;
#12917 = EDGE_CURVE ( 'NONE', #5877, #7271, #9322, .T. ) ;
#12918 = EDGE_LOOP ( 'NONE', ( #13703, #12144, #10506 ) ) ;
#12919 = ORIENTED_EDGE ( 'NONE', *, *, #6512, .F. ) ;
#12920 = ORIENTED_EDGE ( 'NONE', *, *, #4444, .T. ) ;
#12921 = LINE ( 'NONE', #7557, #6074 ) ;
#12922 = DIRECTION ( 'NONE',  ( 0.9960067511297464593, -0.08927794634716622324, 6.802837160686558945E-17 ) ) ;
#12923 = CIRCLE ( 'NONE', #13627, 2.000000000000000000 ) ;
#12924 = FACE_OUTER_BOUND ( 'NONE', #8165, .T. ) ;
#12925 = CARTESIAN_POINT ( 'NONE',  ( 4.066030946031333748, 90.77438413795609051, -2.912544222229247914 ) ) ;
#12926 = CARTESIAN_POINT ( 'NONE',  ( -8.551509863446513648, -93.00797441535850396, -0.1595843423901910085 ) ) ;
#12927 = DIRECTION ( 'NONE',  ( 1.000000000000000000, 0.000000000000000000, 0.000000000000000000 ) ) ;
#12928 = ORIENTED_EDGE ( 'NONE', *, *, #7151, .F. ) ;
#12929 = ORIENTED_EDGE ( 'NONE', *, *, #1891, .T. ) ;
#12930 = VERTEX_POINT ( 'NONE', #12784 ) ;
#12931 = CARTESIAN_POINT ( 'NONE',  ( -2.517691654963332357E-15, 90.00000000000000000, -1.589271161308885878E-16 ) ) ;
#12932 = CARTESIAN_POINT ( 'NONE',  ( -15.29705854078139105, 90.00000000000000000, -1.589271161308885878E-16 ) ) ;
#12933 = EDGE_LOOP ( 'NONE', ( #13649, #4207, #8128, #8514 ) ) ;
#12934 = CARTESIAN_POINT ( 'NONE',  ( -15.29705854078139282, -1.063309978032445979, -1.869594071425719488E-15 ) ) ;
#12935 = CARTESIAN_POINT ( 'NONE',  ( 34.00000000000001421, 108.0000000000000142, -0.5000000000000000000 ) ) ;
#12936 = CARTESIAN_POINT ( 'NONE',  ( -8.385254915620294014, 3.280056672672198914, -5.792110530374064999E-18 ) ) ;
#12937 = DIRECTION ( 'NONE',  ( -6.158143864569485777E-17, -2.736152283717910599E-16, 1.000000000000000000 ) ) ;
#12938 = DIRECTION ( 'NONE',  ( 0.4545454545454548634, 0.8907235428302464619, 0.000000000000000000 ) ) ;
#12939 = CARTESIAN_POINT ( 'NONE',  ( -0.9052951019203371308, -81.00000000000012790, -10.12030223674820562 ) ) ;
#12940 = EDGE_CURVE ( 'NONE', #2529, #6545, #2824, .T. ) ;
#12941 = DIRECTION ( 'NONE',  ( 0.000000000000000000, 0.000000000000000000, 1.000000000000000000 ) ) ;
#12942 = DIRECTION ( 'NONE',  ( 0.6000000000000001998, 0.7999999999999998224, -0.000000000000000000 ) ) ;
#12943 = B_SPLINE_CURVE_WITH_KNOTS ( 'NONE', 3,
 ( #2864, #1678, #10498, #4898, #12622, #12688, #5961, #7204, #12554, #2939, #10299, #9248, #9174, #1880, #1743, #6167, #703, #10435, #837, #12411, #5103, #2998, #11555, #7068, #6297, #13290, #5609, #9056, #12140, #8072, #299, #371, #5827, #738, #1495, #1710, #12302, #7950, #3881, #9077, #2694, #9282, #3665, #10261, #12235, #10057, #6893, #2625, #11378, #5996, #6968, #5001, #11252, #6062, #11179, #12440, #13597, #1565, #666, #8095, #5855, #4934, #12381, #10128, #538, #3949, #13393, #13313, #3807, #1637, #10335, #8224, #12513, #13533, #13464, #5922, #4723, #3742, #5775, #6828, #603, #464, #4866, #9214, #8162, #7034, #11105, #8024, #11313, #10196, #2767, #2831, #9007, #9142, #7103, #11522, #803, #7168, #10598, #2050, #3037, #4011, #11652, #11591, #6258, #5269, #9556, #13864, #1493, #2828, #3662, #664, #3877, #11176, #3740, #5994, #12300, #11250, #12156, #10193, #4798, #5773, #2548, #5853 ),
 .UNSPECIFIED., .F., .F.,
 ( 4, 2, 2, 2, 2, 2, 2, 2, 2, 2, 2, 2, 2, 2, 2, 2, 2, 2, 2, 2, 2, 2, 2, 2, 2, 2, 2, 2, 2, 2, 2, 2, 2, 2, 2, 2, 2, 2, 2, 2, 2, 2, 2, 2, 2, 2, 2, 2, 2, 2, 2, 2, 2, 2, 2, 2, 2, 2, 2, 2, 2, 4 ),
 ( 2.912531104258623014E-17, 0.0008227720497348227488, 0.001645544099469616224, 0.003291088198939203392, 0.004936632298408791426, 0.006582176397878378160, 0.008227720497347964027, 0.009050492547082742215, 0.009873264596817522137, 0.01316435279575666265, 0.01480989689522623463, 0.01645544099469580662, 0.01810098509416537688, 0.01892375714390017935, 0.01974652919363497836, 0.02303761739257425070, 0.02468316149204390075, 0.02632870559151355080, 0.02797424969098320433, 0.02961979379045285438, 0.03291088198939215448, 0.03455642608886181494, 0.03620197018833147540, 0.03784751428780114280, 0.03949305838727080326, 0.04278414658621013111, 0.04360691863594496481, 0.04442969068567979851, 0.04607523478514943122, 0.04772077888461906392, 0.04854355093435388374, 0.04936632298408870356, 0.05101186708355830157, 0.05265741118302790652, 0.05594849938196708172, 0.05759404348143667279, 0.05923958758090627774, 0.06088513168037586881, 0.06253067577984547376, 0.06582176397878466978, 0.06746730807825425391, 0.06911285217772385192, 0.07075839627719342217, 0.07240394037666302018, 0.07569502857560218845, 0.07734057267507175870, 0.07898611677454135671, 0.08063166087401094084, 0.08227720497348053885, 0.08556829317241962385, 0.08721383727188916635, 0.08885938137135870885, 0.09050492547082823747, 0.09215046957029777996, 0.09379601366976733634, 0.09544155776923687884, 0.09708710186870640746, 0.09873264596817596384, 0.1020237341671150488, 0.1036692782665845497, 0.1044920503163192654, 0.1053148223660539812 ),
 .UNSPECIFIED. ) ;
#12944 = VERTEX_POINT ( 'NONE', #1399 ) ;
#12945 = CARTESIAN_POINT ( 'NONE',  ( -35.00000000000000000, -4.286263797015736496E-15, 7.500000000000000000 ) ) ;
#12946 = ORIENTED_EDGE ( 'NONE', *, *, #6719, .F. ) ;
#12947 = CARTESIAN_POINT ( 'NONE',  ( -24.99999999999998934, -99.15310334213020838, 4.530792947966844994E-20 ) ) ;
#12948 = DIRECTION ( 'NONE',  ( -1.000000000000000000, 0.000000000000000000, 0.000000000000000000 ) ) ;
#12949 = VERTEX_POINT ( 'NONE', #12056 ) ;
#12950 = DIRECTION ( 'NONE',  ( 0.000000000000000000, 0.000000000000000000, 1.000000000000000000 ) ) ;
#12951 = ORIENTED_EDGE ( 'NONE', *, *, #4138, .F. ) ;
#12952 = CARTESIAN_POINT ( 'NONE',  ( -12.99579180576517068, 73.50828762700209040, -1.851135709604445740E-15 ) ) ;
#12953 = CARTESIAN_POINT ( 'NONE',  ( 12.99579180576516713, 54.65873172698324112, 1.506871011810438326E-15 ) ) ;
#12954 = CYLINDRICAL_SURFACE ( 'NONE', #4028, 9.000000000008999024 ) ;
#12955 = EDGE_CURVE ( 'NONE', #6325, #1805, #3487, .T. ) ;
#12956 = CARTESIAN_POINT ( 'NONE',  ( -25.00000000000000355, 120.0000000000000142, -0.5000000000000000000 ) ) ;
#12957 = EDGE_CURVE ( 'NONE', #2827, #12412, #7769, .T. ) ;
#12958 = CARTESIAN_POINT ( 'NONE',  ( 34.99999999999958789, 1.104930248025249758E-13, -2.499999999999999112 ) ) ;
#12959 = CYLINDRICAL_SURFACE ( 'NONE', #10151, 15.29705854078139105 ) ;
#12960 = DIRECTION ( 'NONE',  ( -1.000000000000000000, 0.000000000000000000, 0.000000000000000000 ) ) ;
#12961 = VERTEX_POINT ( 'NONE', #13134 ) ;
#12962 = CIRCLE ( 'NONE', #5787, 42.00000000000001421 ) ;
#12963 = ORIENTED_EDGE ( 'NONE', *, *, #5817, .F. ) ;
#12964 = VECTOR ( 'NONE', #12414, 1000.000000000000000 ) ;
#12965 = B_SPLINE_CURVE_WITH_KNOTS ( 'NONE', 3,
 ( #13163, #10872, #4360, #398 ),
 .UNSPECIFIED., .F., .F.,
 ( 4, 4 ),
 ( 0.000000000000000000, 1.000000000000000000 ),
 .UNSPECIFIED. ) ;
#12966 =( NAMED_UNIT ( * ) PLANE_ANGLE_UNIT ( ) SI_UNIT ( $, .RADIAN. ) );
#12967 = ORIENTED_EDGE ( 'NONE', *, *, #10971, .T. ) ;
#12968 = CARTESIAN_POINT ( 'NONE',  ( 0.000000000000000000, 71.01020514433645303, 2.500000000000000000 ) ) ;
#12969 = ADVANCED_FACE ( 'NONE', ( #2447 ), #6405, .F. ) ;
#12970 = CYLINDRICAL_SURFACE ( 'NONE', #8441, 18.74900000001875000 ) ;
#12971 = EDGE_CURVE ( 'NONE', #2573, #8647, #10998, .T. ) ;
#12972 = DIRECTION ( 'NONE',  ( -4.163336342344333082E-15, 1.000000000000000000, 1.734723475976805615E-16 ) ) ;
#12973 = AXIS2_PLACEMENT_3D ( 'NONE', #12748, #4315, #12830 ) ;
#12974 = DIRECTION ( 'NONE',  ( 1.000000000000000000, 0.000000000000000000, 0.000000000000000000 ) ) ;
#12975 = EDGE_CURVE ( 'NONE', #13355, #11738, #6826, .T. ) ;
#12976 = CIRCLE ( 'NONE', #5800, 2.500000000000002220 ) ;
#12977 = ORIENTED_EDGE ( 'NONE', *, *, #1968, .T. ) ;
#12978 = EDGE_CURVE ( 'NONE', #5587, #11767, #7948, .T. ) ;
#12979 = ORIENTED_EDGE ( 'NONE', *, *, #6430, .F. ) ;
#12980 = AXIS2_PLACEMENT_3D ( 'NONE', #9928, #13185, #13334 ) ;
#12981 = ORIENTED_EDGE ( 'NONE', *, *, #7464, .T. ) ;
#12982 = CARTESIAN_POINT ( 'NONE',  ( 10.69381717166375445, 53.83378072214353693, 0.000000000000000000 ) ) ;
#12983 = ORIENTED_EDGE ( 'NONE', *, *, #3189, .F. ) ;
#12984 = LINE ( 'NONE', #75, #3626 ) ;
#12985 = DIRECTION ( 'NONE',  ( 1.000000000000000000, 0.000000000000000000, 0.000000000000000000 ) ) ;
#12986 = CARTESIAN_POINT ( 'NONE',  ( -2.132246523607266586E-15, 76.22148119144830503, -1.345962243664627229E-16 ) ) ;
#12987 = FACE_OUTER_BOUND ( 'NONE', #12264, .T. ) ;
#12988 = CYLINDRICAL_SURFACE ( 'NONE', #10051, 24.99999999999998934 ) ;
#12989 = CARTESIAN_POINT ( 'NONE',  ( 16.29599561779310335, 1.298160649189403548, 2.499999999999999112 ) ) ;
#12990 = ORIENTED_EDGE ( 'NONE', *, *, #10621, .T. ) ;
#12991 = EDGE_CURVE ( 'NONE', #11019, #8296, #2606, .T. ) ;
#12992 = CIRCLE ( 'NONE', #3561, 8.385254915620292238 ) ;
#12993 = EDGE_LOOP ( 'NONE', ( #13747, #5272, #4569, #8472 ) ) ;
#12994 = ORIENTED_EDGE ( 'NONE', *, *, #9112, .F. ) ;
#12995 = AXIS2_PLACEMENT_3D ( 'NONE', #3386, #10752, #1168 ) ;
#12996 = LINE ( 'NONE', #3363, #9615 ) ;
#12997 = LINE ( 'NONE', #3365, #9861 ) ;
#12998 = ORIENTED_EDGE ( 'NONE', *, *, #6798, .F. ) ;
#12999 = CARTESIAN_POINT ( 'NONE',  ( -1.146365672123090463E-15, 40.97916847270985130, -7.236334518677345233E-17 ) ) ;
#13000 = SURFACE_SIDE_STYLE ('',( #8697 ) ) ;
#13001 = CARTESIAN_POINT ( 'NONE',  ( -15.29705854078139282, 36.63580182200523438, -2.002736540738517883E-15 ) ) ;
#13002 = CARTESIAN_POINT ( 'NONE',  ( -15.29705854078139460, -8.601520358636511432, -3.733175406185929791E-15 ) ) ;
#13003 = AXIS2_PLACEMENT_3D ( 'NONE', #2299, #9674, #3149 ) ;
#13004 = CYLINDRICAL_SURFACE ( 'NONE', #11178, 18.74900000001875000 ) ;
#13005 = CARTESIAN_POINT ( 'NONE',  ( -1.483439550716517611E-15, 53.02855864072483882, -9.364084330386787485E-17 ) ) ;
#13006 = AXIS2_PLACEMENT_3D ( 'NONE', #9860, #1371, #8956 ) ;
#13007 = CARTESIAN_POINT ( 'NONE',  ( -6.150798755069114776, -74.45454545454569484, -8.129532795066724660 ) ) ;
#13008 = AXIS2_PLACEMENT_3D ( 'NONE', #3647, #8143, #6945 ) ;
#13009 = DIRECTION ( 'NONE',  ( 0.000000000000000000, 0.000000000000000000, 1.000000000000000000 ) ) ;
#13010 = CYLINDRICAL_SURFACE ( 'NONE', #1202, 8.385254915620292238 ) ;
#13011 = VERTEX_POINT ( 'NONE', #12456 ) ;
#13012 = DIRECTION ( 'NONE',  ( 0.01532218268402011502, -0.9998826084685129567, -2.891205793291787644E-16 ) ) ;
#13013 = FACE_OUTER_BOUND ( 'NONE', #9749, .T. ) ;
#13014 = AXIS2_PLACEMENT_3D ( 'NONE', #12599, #4089, #39 ) ;
#13015 = ORIENTED_EDGE ( 'NONE', *, *, #2347, .T. ) ;
#13016 = AXIS2_PLACEMENT_3D ( 'NONE', #6997, #1670, #629 ) ;
#13017 = CIRCLE ( 'NONE', #6067, 15.29705854078138749 ) ;
#13018 = PLANE ( 'NONE',  #3470 ) ;
#13019 = CARTESIAN_POINT ( 'NONE',  ( -2.517691654963332357E-15, 90.00000000000000000, -1.589271161308885878E-16 ) ) ;
#13020 = ORIENTED_EDGE ( 'NONE', *, *, #1284, .T. ) ;
#13021 = CARTESIAN_POINT ( 'NONE',  ( -4.288313376222440694E-16, 15.32944684068712782, -2.706960864746847057E-17 ) ) ;
#13022 = ORIENTED_EDGE ( 'NONE', *, *, #4114, .T. ) ;
#13023 = LINE ( 'NONE', #5556, #1443 ) ;
#13024 = CARTESIAN_POINT ( 'NONE',  ( -12.99553232110414847, 1.649976794542511671, 25.99106464220827917 ) ) ;
#13025 = CARTESIAN_POINT ( 'NONE',  ( 34.63132358390374321, 107.2645221665701456, -2.217002873864902135 ) ) ;
#13026 = CIRCLE ( 'NONE', #12809, 27.49999999999998579 ) ;
#13027 = CARTESIAN_POINT ( 'NONE',  ( -15.29705854078139993, -19.91286587805129926, 3.516327053222078456E-17 ) ) ;
#13028 = CARTESIAN_POINT ( 'NONE',  ( -8.385254915620290461, 12.70483462268160046, -16.77050983124058803 ) ) ;
#13029 =( REPRESENTATION_RELATIONSHIP ('NONE','NONE', #9450, #1365 ) REPRESENTATION_RELATIONSHIP_WITH_TRANSFORMATION ( #4600 )SHAPE_REPRESENTATION_RELATIONSHIP( ) );
#13030 = DIRECTION ( 'NONE',  ( -0.000000000000000000, -0.000000000000000000, -1.000000000000000000 ) ) ;
#13031 = DIRECTION ( 'NONE',  ( -6.158143864569485777E-17, -2.736152283717910599E-16, 1.000000000000000000 ) ) ;
#13032 = VECTOR ( 'NONE', #4301, 1000.000000000000000 ) ;
#13033 = CARTESIAN_POINT ( 'NONE',  ( 31.81818181818183433, 133.3608531424536920, -0.5000000000000000000 ) ) ;
#13034 = CARTESIAN_POINT ( 'NONE',  ( 47.49999999999999289, 120.0000000000000142, -2.499999999999998668 ) ) ;
#13035 = ORIENTED_EDGE ( 'NONE', *, *, #8742, .T. ) ;
#13036 = DIRECTION ( 'NONE',  ( -0.9960067511297463483, 0.08927794634716618161, -4.818676322152979407E-17 ) ) ;
#13037 = ADVANCED_FACE ( 'NONE', ( #9496 ), #2730, .T. ) ;
#13038 = ORIENTED_EDGE ( 'NONE', *, *, #13423, .T. ) ;
#13039 = DIRECTION ( 'NONE',  ( -2.797435172181481150E-17, 1.000000000000000000, -1.765856845898762549E-18 ) ) ;
#13040 = AXIS2_PLACEMENT_3D ( 'NONE', #13152, #3575, #9690 ) ;
#13041 = DIRECTION ( 'NONE',  ( 0.000000000000000000, 0.000000000000000000, 1.000000000000000000 ) ) ;
#13042 = VERTEX_POINT ( 'NONE', #6070 ) ;
#13043 = DIRECTION ( 'NONE',  ( -2.797435172181481150E-17, 1.000000000000000000, -1.765856845898762549E-18 ) ) ;
#13044 = CARTESIAN_POINT ( 'NONE',  ( 18.54049621773915746, -20.00000000000000000, 7.500000000000000000 ) ) ;
#13045 = CARTESIAN_POINT ( 'NONE',  ( -1.815818965600183303E-15, 64.91013567203349055, -1.146220074446778111E-16 ) ) ;
#13046 = UNCERTAINTY_MEASURE_WITH_UNIT (LENGTH_MEASURE( 1.000000000000000082E-05 ), #12427, 'distance_accuracy_value', 'NONE');
#13047 = DIRECTION ( 'NONE',  ( 1.000000000000000000, 1.009293658750142794E-15, 0.000000000000000000 ) ) ;
#13048 = VERTEX_POINT ( 'NONE', #6211 ) ;
#13049 = PRODUCT_DEFINITION_SHAPE ( 'NONE', 'NONE',  #8055 ) ;
#13050 = ORIENTED_EDGE ( 'NONE', *, *, #2173, .F. ) ;
#13051 = ORIENTED_EDGE ( 'NONE', *, *, #7544, .F. ) ;
#13052 = EDGE_CURVE ( 'NONE', #2949, #11754, #3104, .T. ) ;
#13053 = CARTESIAN_POINT ( 'NONE',  ( -10.00000000000000000, 90.00000000000000000, 0.5000000000000000000 ) ) ;
#13054 = ADVANCED_FACE ( 'NONE', ( #11531 ), #1923, .T. ) ;
#13055 = EDGE_CURVE ( 'NONE', #10090, #6890, #11666, .T. ) ;
#13056 = VERTEX_POINT ( 'NONE', #10541 ) ;
#13057 = ORIENTED_EDGE ( 'NONE', *, *, #12536, .T. ) ;
#13058 = CARTESIAN_POINT ( 'NONE',  ( 43.14708730495711819, 24.16350488746833136, -2.499999999999992450 ) ) ;
#13059 = ORIENTED_EDGE ( 'NONE', *, *, #1706, .T. ) ;
#13060 = ADVANCED_FACE ( 'NONE', ( #3962 ), #8235, .T. ) ;
#13061 = CARTESIAN_POINT ( 'NONE',  ( -12.99579180576517601, 73.50828762700210461, 25.99158361153033070 ) ) ;
#13062 = ADVANCED_FACE ( 'NONE', ( #10472 ), #4343, .F. ) ;
#13063 = CARTESIAN_POINT ( 'NONE',  ( 45.47624229149391084, 15.54906262289183871, -2.499999999999994671 ) ) ;
#13064 = CARTESIAN_POINT ( 'NONE',  ( -4.711442097700778042, -75.83792215129622605, -8.965827225112430909 ) ) ;
#13065 = CARTESIAN_POINT ( 'NONE',  ( 39.10224891377572476, 101.4936815461678350, -2.486392430613897364 ) ) ;
#13066 = CARTESIAN_POINT ( 'NONE',  ( 2.179449471770333435, 90.00000000000000000, -4.500000000000000888 ) ) ;
#13067 = CARTESIAN_POINT ( 'NONE',  ( -7.108720426521072611, -96.49446529545537032, -3.837650603676977301 ) ) ;
#13068 = LINE ( 'NONE', #3424, #785 ) ;
#13069 = ORIENTED_EDGE ( 'NONE', *, *, #7625, .F. ) ;
#13070 = EDGE_LOOP ( 'NONE', ( #13022, #6456, #2652, #11536 ) ) ;
#13071 = ORIENTED_EDGE ( 'NONE', *, *, #12193, .T. ) ;
#13072 = AXIS2_PLACEMENT_3D ( 'NONE', #11953, #2344, #4590 ) ;
#13073 = EDGE_CURVE ( 'NONE', #9516, #6752, #2143, .T. ) ;
#13074 = CARTESIAN_POINT ( 'NONE',  ( 26.69171018101576465, -19.44228176112429551, -2.500000000000004441 ) ) ;
#13075 = DIRECTION ( 'NONE',  ( -0.000000000000000000, -0.000000000000000000, -1.000000000000000000 ) ) ;
#13076 = ORIENTED_EDGE ( 'NONE', *, *, #7270, .F. ) ;
#13077 = DIRECTION ( 'NONE',  ( -1.000000000000000000, -1.224646799147353207E-16, 0.000000000000000000 ) ) ;
#13078 = SHAPE_REPRESENTATION_RELATIONSHIP ( 'NONE' , 'NONE' ,  #2342, #11412 ) ;
#13079 = CYLINDRICAL_SURFACE ( 'NONE', #130, 9.000000000008999024 ) ;
#13080 = EDGE_CURVE ( 'NONE', #11053, #2573, #1704, .T. ) ;
#13081 = CARTESIAN_POINT ( 'NONE',  ( -8.385254915620288685, 5.904668890677672088, -16.77050983124058448 ) ) ;
#13082 = CIRCLE ( 'NONE', #1641, 5.000000000000004441 ) ;
#13083 = CARTESIAN_POINT ( 'NONE',  ( 2.491129965231927645, -148.3982683980968034, -1.520867222960365472 ) ) ;
#13084 = FACE_OUTER_BOUND ( 'NONE', #7730, .T. ) ;
#13085 = CARTESIAN_POINT ( 'NONE',  ( -1.238635481694431384, -80.00117812811808449, -9.950197937997891984 ) ) ;
#13086 = DIRECTION ( 'NONE',  ( 1.000000000000000000, 0.000000000000000000, 0.000000000000000000 ) ) ;
#13087 = CARTESIAN_POINT ( 'NONE',  ( -2.197875741315214793, -79.21212121212059287, -9.798460318839479655 ) ) ;
#13088 = DIRECTION ( 'NONE',  ( 0.6000000000000001998, -0.7999999999999998224, -0.000000000000000000 ) ) ;
#13089 = FACE_OUTER_BOUND ( 'NONE', #10662, .T. ) ;
#13090 = EDGE_LOOP ( 'NONE', ( #4655, #12108, #4646, #13458 ) ) ;
#13091 = VECTOR ( 'NONE', #12942, 999.9999999999998863 ) ;
#13092 = DIRECTION ( 'NONE',  ( -1.000000000000000000, 0.000000000000000000, 0.000000000000000000 ) ) ;
#13093 = CARTESIAN_POINT ( 'NONE',  ( -8.385254915620286909, 71.87811454074363837, -16.77050983124057737 ) ) ;
#13094 = VERTEX_POINT ( 'NONE', #3046 ) ;
#13095 = CARTESIAN_POINT ( 'NONE',  ( 15.18222645069203125, -100.0000000000000000, -4.000000000000000000 ) ) ;
#13096 = DIRECTION ( 'NONE',  ( -2.797435172181479917E-17, 1.000000000000000000, -1.765856845898779112E-18 ) ) ;
#13097 = ORIENTED_EDGE ( 'NONE', *, *, #3023, .F. ) ;
#13098 = DIRECTION ( 'NONE',  ( -1.000000000000000000, 0.000000000000000000, 0.000000000000000000 ) ) ;
#13099 = DIRECTION ( 'NONE',  ( 1.224646799147353207E-16, 1.000000000000000000, -0.000000000000000000 ) ) ;
#13100 = CARTESIAN_POINT ( 'NONE',  ( 8.385254915620290461, 24.75422479069652937, 16.77050983124058803 ) ) ;
#13101 = DIRECTION ( 'NONE',  ( 0.000000000000000000, 0.000000000000000000, 1.000000000000000000 ) ) ;
#13102 = CARTESIAN_POINT ( 'NONE',  ( -2.517691654963332357E-15, 90.00000000000000000, -1.589271161308885878E-16 ) ) ;
#13103 = DIRECTION ( 'NONE',  ( 0.000000000000000000, 0.000000000000000000, 1.000000000000000000 ) ) ;
#13104 = DIRECTION ( 'NONE',  ( -1.000000000000000000, 0.000000000000000000, 0.000000000000000000 ) ) ;
#13105 = DIRECTION ( 'NONE',  ( 0.000000000000000000, 0.000000000000000000, 1.000000000000000000 ) ) ;
#13106 = EDGE_LOOP ( 'NONE', ( #3966, #7913 ) ) ;
#13107 = ORIENTED_EDGE ( 'NONE', *, *, #10054, .F. ) ;
#13108 = VECTOR ( 'NONE', #2531, 1000.000000000000000 ) ;
#13109 = VERTEX_POINT ( 'NONE', #2322 ) ;
#13110 = CARTESIAN_POINT ( 'NONE',  ( 10.00000000000000711, 139.9999999999999716, 0.5000000000000000000 ) ) ;
#13111 = ORIENTED_EDGE ( 'NONE', *, *, #5060, .F. ) ;
#13112 = CARTESIAN_POINT ( 'NONE',  ( 35.06230589874905945, 106.5835921350012683, -2.499999999999999556 ) ) ;
#13113 = AXIS2_PLACEMENT_3D ( 'NONE', #10486, #10558, #12820 ) ;
#13114 = CARTESIAN_POINT ( 'NONE',  ( -35.00000000000000000, -4.286263797015736496E-15, 7.500000000000000000 ) ) ;
#13115 = EDGE_CURVE ( 'NONE', #12645, #2744, #1274, .T. ) ;
#13116 = CARTESIAN_POINT ( 'NONE',  ( -2.517691654963332357E-15, 90.00000000000000000, -1.589271161308885878E-16 ) ) ;
#13117 = VECTOR ( 'NONE', #4431, 1000.000000000000000 ) ;
#13118 = EDGE_LOOP ( 'NONE', ( #4719, #136, #6205, #13480 ) ) ;
#13119 = CARTESIAN_POINT ( 'NONE',  ( -12.99553232110413781, -26.62435705548576692, -25.99106464220828627 ) ) ;
#13120 = VECTOR ( 'NONE', #2128, 1000.000000000000000 ) ;
#13121 = ORIENTED_EDGE ( 'NONE', *, *, #11075, .F. ) ;
#13122 = LINE ( 'NONE', #4537, #697 ) ;
#13123 = AXIS2_PLACEMENT_3D ( 'NONE', #5203, #2382, #8769 ) ;
#13124 = VERTEX_POINT ( 'NONE', #12002 ) ;
#13125 = CARTESIAN_POINT ( 'NONE',  ( -35.45454545454546036, 140.4866414850956460, 0.5000000000000000000 ) ) ;
#13126 = AXIS2_PLACEMENT_3D ( 'NONE', #9070, #6820, #12077 ) ;
#13127 = CYLINDRICAL_SURFACE ( 'NONE', #4897, 14.99999999999999112 ) ;
#13128 = CARTESIAN_POINT ( 'NONE',  ( -38.79999999999999716, 101.5999999999999943, 2.500000000000000000 ) ) ;
#13129 = FACE_OUTER_BOUND ( 'NONE', #3185, .T. ) ;
#13130 = CARTESIAN_POINT ( 'NONE',  ( 4.330127018922190985, 92.00000000000000000, -2.500000000000000000 ) ) ;
#13131 = EDGE_CURVE ( 'NONE', #12240, #4671, #8432, .T. ) ;
#13132 = CARTESIAN_POINT ( 'NONE',  ( -12.99579180576516713, -30.16426982310158422, -25.99158361153034491 ) ) ;
#13133 = ADVANCED_FACE ( 'NONE', ( #8504 ), #3388, .F. ) ;
#13134 = CARTESIAN_POINT ( 'NONE',  ( -21.99999999999997868, -100.0000000000000000, 0.000000000000000000 ) ) ;
#13135 = AXIS2_PLACEMENT_3D ( 'NONE', #7160, #9346, #6194 ) ;
#13136 = VERTEX_POINT ( 'NONE', #6155 ) ;
#13137 = PRODUCT_DEFINITION_FORMATION_WITH_SPECIFIED_SOURCE ( 'ANY', '', #9897, .NOT_KNOWN. ) ;
#13138 = ORIENTED_EDGE ( 'NONE', *, *, #5395, .T. ) ;
#13139 = EDGE_CURVE ( 'NONE', #369, #1961, #4037, .T. ) ;
#13140 = VECTOR ( 'NONE', #8826, 1000.000000000000000 ) ;
#13141 = EDGE_CURVE ( 'NONE', #2577, #6733, #12207, .T. ) ;
#13142 = ORIENTED_EDGE ( 'NONE', *, *, #6132, .F. ) ;
#13143 = CARTESIAN_POINT ( 'NONE',  ( -8.385254915620292238, 5.904668890677672088, -1.042679998336861873E-17 ) ) ;
#13144 = CARTESIAN_POINT ( 'NONE',  ( 26.69171018101576465, -19.44228176112429551, 2.499999999999994227 ) ) ;
#13145 = ORIENTED_EDGE ( 'NONE', *, *, #10458, .F. ) ;
#13146 = CARTESIAN_POINT ( 'NONE',  ( -12.99579180576517068, -1.889935973073298747, 25.99158361153033070 ) ) ;
#13147 = AXIS2_PLACEMENT_3D ( 'NONE', #656, #2963, #10395 ) ;
#13148 = CARTESIAN_POINT ( 'NONE',  ( 0.000000000000000000, 0.000000000000000000, 0.000000000000000000 ) ) ;
#13149 = CARTESIAN_POINT ( 'NONE',  ( -8.385254915620292238, 34.17900274070598243, 16.77050983124057382 ) ) ;
#13150 = DIRECTION ( 'NONE',  ( 0.000000000000000000, 0.000000000000000000, 1.000000000000000000 ) ) ;
#13151 = CARTESIAN_POINT ( 'NONE',  ( -0.5797347049570008570, -122.9090909090927113, 5.796875383663884662 ) ) ;
#13152 = CARTESIAN_POINT ( 'NONE',  ( 34.99999999999958789, 1.091249486606660213E-13, 2.500000000000000000 ) ) ;
#13153 = CARTESIAN_POINT ( 'NONE',  ( -0.09220535797252617238, -163.8787878627269095, 3.538661136716170219 ) ) ;
#13154 = CARTESIAN_POINT ( 'NONE',  ( -11.81226048336476708, -40.00941361824963849, -1.520867253700650540E-15 ) ) ;
#13155 = DIRECTION ( 'NONE',  ( 1.224646799147353207E-16, -1.000000000000000000, 0.000000000000000000 ) ) ;
#13156 = ADVANCED_FACE ( 'NONE', ( #689, #3761 ), #1733, .T. ) ;
#13157 = DIRECTION ( 'NONE',  ( 0.000000000000000000, -0.000000000000000000, 1.000000000000000000 ) ) ;
#13158 = AXIS2_PLACEMENT_3D ( 'NONE', #11055, #10012, #8966 ) ;
#13159 = ORIENTED_EDGE ( 'NONE', *, *, #2094, .T. ) ;
#13160 = VERTEX_POINT ( 'NONE', #6015 ) ;
#13161 = EDGE_CURVE ( 'NONE', #9616, #8450, #7733, .T. ) ;
#13162 = EDGE_CURVE ( 'NONE', #5237, #13265, #9434, .T. ) ;
#13163 = CARTESIAN_POINT ( 'NONE',  ( 8.385254915620294014, 3.280056672672199358, 1.018788103988028997E-15 ) ) ;
#13164 = DIRECTION ( 'NONE',  ( -0.8735848310779960046, 0.4866719047884612293, 9.637352644305955116E-17 ) ) ;
#13165 = ORIENTED_EDGE ( 'NONE', *, *, #6701, .T. ) ;
#13166 = CYLINDRICAL_SURFACE ( 'NONE', #11888, 18.74900000001875000 ) ;
#13167 = DIRECTION ( 'NONE',  ( -0.000000000000000000, -0.000000000000000000, 1.000000000000000000 ) ) ;
#13168 = DIRECTION ( 'NONE',  ( -1.000000000000000000, 0.000000000000000000, 0.000000000000000000 ) ) ;
#13169 = ORIENTED_EDGE ( 'NONE', *, *, #2347, .F. ) ;
#13170 = ORIENTED_EDGE ( 'NONE', *, *, #3015, .T. ) ;
#13171 = CARTESIAN_POINT ( 'NONE',  ( 15.29705854078138749, 10.24803554138234496, 1.856918518244839783E-15 ) ) ;
#13172 = ORIENTED_EDGE ( 'NONE', *, *, #9008, .T. ) ;
#13173 = DIRECTION ( 'NONE',  ( -0.000000000000000000, -0.000000000000000000, -1.000000000000000000 ) ) ;
#13174 = CARTESIAN_POINT ( 'NONE',  ( -2.517691654963332357E-15, 90.00000000000000000, -1.589271161308885878E-16 ) ) ;
#13175 = AXIS2_PLACEMENT_3D ( 'NONE', #5871, #10144, #13407 ) ;
#13176 = DIRECTION ( 'NONE',  ( 0.000000000000000000, -1.000000000000000000, 0.000000000000000000 ) ) ;
#13177 = DIRECTION ( 'NONE',  ( -2.797435172181481150E-17, 1.000000000000000000, -1.765856845898762549E-18 ) ) ;
#13178 = PRODUCT_DEFINITION_SHAPE ( 'NONE', 'NONE',  #4712 ) ;
#13179 = DIRECTION ( 'NONE',  ( -0.6000000000000001998, 0.7999999999999998224, 0.000000000000000000 ) ) ;
#13180 = CARTESIAN_POINT ( 'NONE',  ( -15.29705854078138927, 66.79670324143890525, -1.179534157023628988E-16 ) ) ;
#13181 = EDGE_CURVE ( 'NONE', #7055, #3625, #9375, .T. ) ;
#13182 = CARTESIAN_POINT ( 'NONE',  ( -10.04421448780857062, -71.03329039521169364, -1.233851563443314925 ) ) ;
#13183 = CARTESIAN_POINT ( 'NONE',  ( -8.385254915620295790, -31.79444290936001494, 16.77050983124058803 ) ) ;
#13184 = DIRECTION ( 'NONE',  ( -6.158143864569485777E-17, -2.736152283717910599E-16, 1.000000000000000000 ) ) ;
#13185 = DIRECTION ( 'NONE',  ( -0.8907235428302473501, -0.4545454545454531425, 0.000000000000000000 ) ) ;
#13186 = ADVANCED_FACE ( 'NONE', ( #4957 ), #12243, .T. ) ;
#13187 = EDGE_LOOP ( 'NONE', ( #8333, #9820, #13766, #3511, #3250, #6807, #12752, #13199, #13651, #5852 ) ) ;
#13188 = EDGE_LOOP ( 'NONE', ( #5448, #6869, #8196, #8335 ) ) ;
#13189 = CARTESIAN_POINT ( 'NONE',  ( 35.00000000000009237, 91.25000000000046896, -4.000000000000000000 ) ) ;
#13190 = APPLICATION_PROTOCOL_DEFINITION ( 'draft international standard', 'automotive_design', 1998, #10837 ) ;
#13191 = ORIENTED_EDGE ( 'NONE', *, *, #5865, .T. ) ;
#13192 = DIRECTION ( 'NONE',  ( 0.9960067511297463483, -0.08927794634716618161, 4.818676322152979407E-17 ) ) ;
#13193 = DIRECTION ( 'NONE',  ( -6.158143864569485777E-17, -2.736152283717910599E-16, 1.000000000000000000 ) ) ;
#13194 = TOROIDAL_SURFACE ( 'NONE', #7995, 22.49999999999999289, 5.000000000000000000 ) ;
#13195 = CARTESIAN_POINT ( 'NONE',  ( 58.40844909094411719, 10.11407490371516182, 4.770489558936219510E-15 ) ) ;
#13196 = CARTESIAN_POINT ( 'NONE',  ( -39.00000000000000000, -4.898587196589413026E-15, -10.49999999999999822 ) ) ;
#13197 = UNCERTAINTY_MEASURE_WITH_UNIT (LENGTH_MEASURE( 1.000000000000000082E-05 ), #9657, 'distance_accuracy_value', 'NONE');
#13198 = CARTESIAN_POINT ( 'NONE',  ( 42.16244658108817589, 105.4500712252157655, 7.500000000000000000 ) ) ;
#13199 = ORIENTED_EDGE ( 'NONE', *, *, #9932, .T. ) ;
#13200 = DIRECTION ( 'NONE',  ( 1.000000000000000000, 0.000000000000000000, 0.000000000000000000 ) ) ;
#13201 = ORIENTED_EDGE ( 'NONE', *, *, #13614, .T. ) ;
#13202 = VECTOR ( 'NONE', #3418, 1000.000000000000000 ) ;
#13203 = CARTESIAN_POINT ( 'NONE',  ( -15.29705854078139460, -27.45107625865536605, -3.726038954167064142E-15 ) ) ;
#13204 = ORIENTED_EDGE ( 'NONE', *, *, #3429, .F. ) ;
#13205 = EDGE_LOOP ( 'NONE', ( #9707, #8144, #2402, #10988, #11674 ) ) ;
#13206 = DIRECTION ( 'NONE',  ( 0.000000000000000000, -0.000000000000000000, 1.000000000000000000 ) ) ;
#13207 = CIRCLE ( 'NONE', #6902, 2.500000000000000444 ) ;
#13208 = CARTESIAN_POINT ( 'NONE',  ( -12.99553232110414136, 77.04820039461787928, -1.863605890287647356E-15 ) ) ;
#13209 = CARTESIAN_POINT ( 'NONE',  ( -9.736331930512843513, -69.99978782402621391, -2.722951059031194276 ) ) ;
#13210 = CIRCLE ( 'NONE', #1097, 25.50000000002550138 ) ;
#13211 = CARTESIAN_POINT ( 'NONE',  ( 89.49979561504950709, -156.1132911148542917, 2.500000000000000000 ) ) ;
#13212 = CARTESIAN_POINT ( 'NONE',  ( 34.99999999999958789, 1.104930248025249758E-13, -2.499999999999999112 ) ) ;
#13213 = DIRECTION ( 'NONE',  ( 0.9960067511297463483, -0.08927794634716619548, 0.000000000000000000 ) ) ;
#13214 = ORIENTED_EDGE ( 'NONE', *, *, #11775, .T. ) ;
#13215 = ORIENTED_EDGE ( 'NONE', *, *, #2363, .F. ) ;
#13216 = ORIENTED_EDGE ( 'NONE', *, *, #9693, .F. ) ;
#13217 = AXIS2_PLACEMENT_3D ( 'NONE', #3912, #8192, #12475 ) ;
#13218 = EDGE_CURVE ( 'NONE', #11359, #1146, #13416, .T. ) ;
#13219 = CARTESIAN_POINT ( 'NONE',  ( -10.69346802281034847, -25.79937747632526879, 21.38693604562068984 ) ) ;
#13220 = AXIS2_PLACEMENT_3D ( 'NONE', #4737, #1577, #9016 ) ;
#13221 = EDGE_CURVE ( 'NONE', #8935, #11003, #11332, .T. ) ;
#13222 = CARTESIAN_POINT ( 'NONE',  ( 9.997547090296855288, -68.99999999999997158, 0.6397344882394334631 ) ) ;
#13223 = VERTEX_POINT ( 'NONE', #625 ) ;
#13224 = CYLINDRICAL_SURFACE ( 'NONE', #2778, 15.29705854078139993 ) ;
#13225 = CARTESIAN_POINT ( 'NONE',  ( 15.29705854078139105, -36.87585420866476227, 1.940132561565339224E-15 ) ) ;
#13226 = CARTESIAN_POINT ( 'NONE',  ( -8.385254915620292238, 43.60378069071538221, -7.699803463976802609E-17 ) ) ;
#13227 = DIRECTION ( 'NONE',  ( -1.000000000000000000, 0.000000000000000000, 0.000000000000000000 ) ) ;
#13228 = CARTESIAN_POINT ( 'NONE',  ( 8.597717047226394627, -85.78354978353216609, -6.129448613119037326 ) ) ;
#13229 = FACE_OUTER_BOUND ( 'NONE', #9025, .T. ) ;
#13230 = CIRCLE ( 'NONE', #1110, 9.000000000008999024 ) ;
#13231 = CARTESIAN_POINT ( 'NONE',  ( 4.974937185533097050, 90.00000000000000000, -0.5000000000000000000 ) ) ;
#13232 = PLANE ( 'NONE',  #11553 ) ;
#13233 = ORIENTED_EDGE ( 'NONE', *, *, #13519, .T. ) ;
#13234 = ORIENTED_EDGE ( 'NONE', *, *, #5842, .T. ) ;
#13235 = VECTOR ( 'NONE', #2695, 1000.000000000000000 ) ;
#13236 = ORIENTED_EDGE ( 'NONE', *, *, #12441, .T. ) ;
#13237 = CARTESIAN_POINT ( 'NONE',  ( 30.72062512117245703, 25.13835616439070719, 4.000000000000000000 ) ) ;
#13238 = ORIENTED_EDGE ( 'NONE', *, *, #9562, .T. ) ;
#13239 = CARTESIAN_POINT ( 'NONE',  ( -34.24999999999972999, -135.0000000000000000, -4.194415287079653581E-15 ) ) ;
#13240 = EDGE_CURVE ( 'NONE', #6890, #12810, #6859, .T. ) ;
#13241 = DIRECTION ( 'NONE',  ( 0.9960067511297463483, -0.08927794634716618161, 4.818676322152979407E-17 ) ) ;
#13242 = AXIS2_PLACEMENT_3D ( 'NONE', #9430, #1081, #3502 ) ;
#13243 = EDGE_CURVE ( 'NONE', #3719, #12240, #8637, .T. ) ;
#13244 = LINE ( 'NONE', #250, #11216 ) ;
#13245 = DIRECTION ( 'NONE',  ( 0.8907235428302473501, -0.4545454545454531425, 0.000000000000000000 ) ) ;
#13246 = ORIENTED_EDGE ( 'NONE', *, *, #9523, .F. ) ;
#13247 = EDGE_CURVE ( 'NONE', #4278, #2799, #147, .T. ) ;
#13248 = DIRECTION ( 'NONE',  ( -0.000000000000000000, 1.000000000000000000, -0.000000000000000000 ) ) ;
#13249 = VECTOR ( 'NONE', #181, 1000.000000000000000 ) ;
#13250 = CARTESIAN_POINT ( 'NONE',  ( 4.330127018922190985, 92.00000000000000000, -2.500000000000000000 ) ) ;
#13251 = CARTESIAN_POINT ( 'NONE',  ( -15.29705854078139282, 46.06057977201469100, -3.826369441655158758E-15 ) ) ;
#13252 = EDGE_CURVE ( 'NONE', #430, #10377, #12916, .T. ) ;
#13253 = DIRECTION ( 'NONE',  ( -0.000000000000000000, -0.000000000000000000, -1.000000000000000000 ) ) ;
#13254 = EDGE_CURVE ( 'NONE', #11542, #3469, #9763, .T. ) ;
#13255 = DIRECTION ( 'NONE',  ( -0.000000000000000000, -0.000000000000000000, -1.000000000000000000 ) ) ;
#13256 = CARTESIAN_POINT ( 'NONE',  ( -0.6173387890061953209, 90.00000000000000000, 4.961742921553712549 ) ) ;
#13257 = CARTESIAN_POINT ( 'NONE',  ( -8.235865139535142987, -74.54711635784300938, -5.866162687843151424 ) ) ;
#13258 = DIRECTION ( 'NONE',  ( -6.158143864569485777E-17, -2.736152283717910599E-16, 1.000000000000000000 ) ) ;
#13259 = PLANE ( 'NONE',  #11028 ) ;
#13260 = AXIS2_PLACEMENT_3D ( 'NONE', #9692, #8701, #2321 ) ;
#13261 = DIRECTION ( 'NONE',  ( 0.9960067511297463483, -0.08927794634716618161, 4.818676322152979407E-17 ) ) ;
#13262 = VECTOR ( 'NONE', #2411, 1000.000000000000000 ) ;
#13263 = CIRCLE ( 'NONE', #6731, 25.00000000000000711 ) ;
#13264 = CARTESIAN_POINT ( 'NONE',  ( -5.503342039658565452E-16, 19.67281349139174296, -3.473937238186366113E-17 ) ) ;
#13265 = VERTEX_POINT ( 'NONE', #12401 ) ;
#13266 = CARTESIAN_POINT ( 'NONE',  ( 14.53672965213156942, 15.21527412409548852, -2.499999999999996447 ) ) ;
#13267 = ADVANCED_FACE ( 'NONE', ( #5292 ), #10556, .F. ) ;
#13268 = EDGE_LOOP ( 'NONE', ( #5958, #4779, #6180, #10355, #8690 ) ) ;
#13269 = DIRECTION ( 'NONE',  ( -0.000000000000000000, -0.000000000000000000, -1.000000000000000000 ) ) ;
#13270 = SHAPE_DEFINITION_REPRESENTATION ( #6764, #9450 ) ;
#13271 = ORIENTED_EDGE ( 'NONE', *, *, #1742, .F. ) ;
#13272 = CARTESIAN_POINT ( 'NONE',  ( 15.29705854078138927, 36.63580182200523438, 1.806990092252540434E-15 ) ) ;
#13273 = ADVANCED_FACE ( 'NONE', ( #9573 ), #6223, .F. ) ;
#13274 = VECTOR ( 'NONE', #9669, 1000.000000000000000 ) ;
#13275 = AXIS2_PLACEMENT_3D ( 'NONE', #8054, #1311, #10092 ) ;
#13276 = FACE_OUTER_BOUND ( 'NONE', #3252, .T. ) ;
#13277 = CARTESIAN_POINT ( 'NONE',  ( 8.385254915620288685, 22.12961257269105531, 16.77050983124058448 ) ) ;
#13278 = FILL_AREA_STYLE_COLOUR ( '', #2277 ) ;
#13279 = ORIENTED_EDGE ( 'NONE', *, *, #1064, .F. ) ;
#13280 = AXIS2_PLACEMENT_3D ( 'NONE', #6266, #6209, #2184 ) ;
#13281 = VECTOR ( 'NONE', #6411, 1000.000000000000000 ) ;
#13282 = ORIENTED_EDGE ( 'NONE', *, *, #6804, .T. ) ;
#13283 = CARTESIAN_POINT ( 'NONE',  ( 12.99553232110412893, 77.04820039461787928, 25.99106464220827561 ) ) ;
#13284 = LINE ( 'NONE', #1395, #3128 ) ;
#13285 = CIRCLE ( 'NONE', #6096, 8.385254915620295790 ) ;
#13286 = CARTESIAN_POINT ( 'NONE',  ( -34.25812584745457201, 108.1980041606221192, 0.5000000000000000000 ) ) ;
#13287 = CARTESIAN_POINT ( 'NONE',  ( -0.4532106388231725846, -104.8728397088437134, 7.045281447031682909 ) ) ;
#13288 = CARTESIAN_POINT ( 'NONE',  ( -12.99579180576516002, 16.95961992694555676, -25.99158361153033070 ) ) ;
#13289 = EDGE_LOOP ( 'NONE', ( #12698, #2557, #5681, #6222 ) ) ;
#13290 = CARTESIAN_POINT ( 'NONE',  ( -8.751592884076366374, -90.91481115778101696, -0.6498984818527145935 ) ) ;
#13291 = CARTESIAN_POINT ( 'NONE',  ( 10.69346802281034314, -6.949821576306441706, 21.38693604562069694 ) ) ;
#13292 = PRODUCT ( 'BR-824', 'BR-824', '', ( #13378 ) ) ;
#13293 = EDGE_LOOP ( 'NONE', ( #5863, #7223, #937, #10578 ) ) ;
#13294 = AXIS2_PLACEMENT_3D ( 'NONE', #8302, #12519, #6138 ) ;
#13295 = CARTESIAN_POINT ( 'NONE',  ( -35.20000000000000995, 106.3999999999999915, 2.500000000000000000 ) ) ;
#13296 = CARTESIAN_POINT ( 'NONE',  ( 10.14773761995948753, -69.33333333333402493, -0.3621078539016990283 ) ) ;
#13297 = ORIENTED_EDGE ( 'NONE', *, *, #3242, .T. ) ;
#13298 = DIRECTION ( 'NONE',  ( 1.000000000000000000, 0.000000000000000000, 0.000000000000000000 ) ) ;
#13299 = CARTESIAN_POINT ( 'NONE',  ( -10.00000000000000711, 139.9999999999999716, 2.500000000000000000 ) ) ;
#13300 = CARTESIAN_POINT ( 'NONE',  ( 12.99553232110414314, -36.04913500549519512, 0.000000000000000000 ) ) ;
#13301 = DIRECTION ( 'NONE',  ( 1.000000000000000000, 0.000000000000000000, 0.000000000000000000 ) ) ;
#13302 = CARTESIAN_POINT ( 'NONE',  ( 25.00000000000000355, 120.0000000000000142, 0.5000000000000000000 ) ) ;
#13303 = CARTESIAN_POINT ( 'NONE',  ( 1.553027081813024735, -81.93939393942123672, -9.741774319690060580 ) ) ;
#13304 = DIRECTION ( 'NONE',  ( 0.9960067511297464593, -0.08927794634716622324, 3.401418580343279473E-17 ) ) ;
#13305 = CARTESIAN_POINT ( 'NONE',  ( -35.00000000000000000, -4.286263797015736496E-15, -4.000000000000000000 ) ) ;
#13306 = CARTESIAN_POINT ( 'NONE',  ( 1.387778780781445676E-14, -135.0000000000000000, 0.000000000000000000 ) ) ;
#13307 = EDGE_LOOP ( 'NONE', ( #6095, #8802, #3066, #9658 ) ) ;
#13308 = ORIENTED_EDGE ( 'NONE', *, *, #8360, .T. ) ;
#13309 = EDGE_CURVE ( 'NONE', #2284, #12537, #2197, .T. ) ;
#13310 = VERTEX_POINT ( 'NONE', #9508 ) ;
#13311 = CARTESIAN_POINT ( 'NONE',  ( -35.06230589874905235, 106.5835921350012825, -2.499999999999999556 ) ) ;
#13312 = ORIENTED_EDGE ( 'NONE', *, *, #4364, .F. ) ;
#13313 = CARTESIAN_POINT ( 'NONE',  ( 5.365047425320059737, -115.1629361961574318, 2.316356917355964384 ) ) ;
#13314 = B_SPLINE_CURVE_WITH_KNOTS ( 'NONE', 3,
 ( #4662, #9786, #2340, #12894 ),
 .UNSPECIFIED., .F., .F.,
 ( 4, 4 ),
 ( 0.000000000000000000, 1.000000000000000000 ),
 .UNSPECIFIED. ) ;
#13315 = CARTESIAN_POINT ( 'NONE',  ( -4.330127018922195425, 92.00000000000000000, -2.500000000000000000 ) ) ;
#13316 = AXIS2_PLACEMENT_3D ( 'NONE', #3622, #7830, #5955 ) ;
#13317 = DIRECTION ( 'NONE',  ( 1.000000000000000000, 0.000000000000000000, 0.000000000000000000 ) ) ;
#13318 = AXIS2_PLACEMENT_3D ( 'NONE', #5644, #13892, #12829 ) ;
#13319 = ORIENTED_EDGE ( 'NONE', *, *, #9601, .T. ) ;
#13320 = CARTESIAN_POINT ( 'NONE',  ( 10.69381717166375800, -12.13966492792242846, 0.000000000000000000 ) ) ;
#13321 = ORIENTED_EDGE ( 'NONE', *, *, #13612, .T. ) ;
#13322 = CARTESIAN_POINT ( 'NONE',  ( -1.386339613915927416, -154.8029363165078962, -0.8714183873244492062 ) ) ;
#13323 = DIRECTION ( 'NONE',  ( -1.000000000000000000, 0.000000000000000000, 0.000000000000000000 ) ) ;
#13324 = FACE_OUTER_BOUND ( 'NONE', #2766, .T. ) ;
#13325 = AXIS2_PLACEMENT_3D ( 'NONE', #8859, #3272, #4118 ) ;
#13326 = DIRECTION ( 'NONE',  ( -1.000000000000000000, 0.000000000000000000, 0.000000000000000000 ) ) ;
#13327 = CARTESIAN_POINT ( 'NONE',  ( -39.95570474821490592, 100.9618745346225523, -2.097587229781390228 ) ) ;
#13328 = CIRCLE ( 'NONE', #7239, 18.74900000001875000 ) ;
#13329 = CARTESIAN_POINT ( 'NONE',  ( 32.72727272727274084, 135.1423002281141805, -0.5000000000000000000 ) ) ;
#13330 =( BOUNDED_SURFACE ( )  B_SPLINE_SURFACE ( 3, 3, ( 
 ( #2583, #6862, #11138, #5809 ),
 ( #13352, #3699, #12263, #2650 ),
 ( #6921, #1603, #6093, #10431 ),
 ( #6293, #7134, #4110, #8392 ) ),
 .UNSPECIFIED., .F., .F., .T. ) 
 B_SPLINE_SURFACE_WITH_KNOTS ( ( 4, 4 ),
 ( 4, 4 ),
 ( 0.000000000000000000, 1.000000000000000000 ),
 ( 0.000000000000000000, 1.000000000000000000 ),
 .UNSPECIFIED. ) 
 GEOMETRIC_REPRESENTATION_ITEM ( )  RATIONAL_B_SPLINE_SURFACE ( (
 ( 1.000000000000000000, 0.3333333333333334259, 0.3333333333333334259, 1.000000000000000000),
 ( 1.000000000000000000, 0.3333333333333334259, 0.3333333333333334259, 1.000000000000000000),
 ( 1.000000000000000000, 0.3333333333333334259, 0.3333333333333334259, 1.000000000000000000),
 ( 1.000000000000000000, 0.3333333333333334259, 0.3333333333333334259, 1.000000000000000000) ) ) 
 REPRESENTATION_ITEM ( '' )  SURFACE ( )  );
#13331 = CARTESIAN_POINT ( 'NONE',  ( 8.385254915620294014, -24.99427717735608212, 1.068716529980328543E-15 ) ) ;
#13332 = EDGE_CURVE ( 'NONE', #12944, #12643, #8518, .T. ) ;
#13333 = CIRCLE ( 'NONE', #9041, 4.999999999999998224 ) ;
#13334 = DIRECTION ( 'NONE',  ( 0.4545454545454531425, -0.8907235428302472391, 0.000000000000000000 ) ) ;
#13335 = EDGE_CURVE ( 'NONE', #1662, #7167, #5280, .T. ) ;
#13336 = EDGE_CURVE ( 'NONE', #10177, #5287, #7074, .T. ) ;
#13337 = ORIENTED_EDGE ( 'NONE', *, *, #10210, .F. ) ;
#13338 = CARTESIAN_POINT ( 'NONE',  ( 11.72298137502706439, -61.00000000000002842, 2.970135970080976850 ) ) ;
#13339 = EDGE_CURVE ( 'NONE', #13647, #1226, #13819, .T. ) ;
#13340 = ADVANCED_FACE ( 'NONE', ( #9708 ), #11533, .T. ) ;
#13341 = ORIENTED_EDGE ( 'NONE', *, *, #13519, .F. ) ;
#13342 = CIRCLE ( 'NONE', #7250, 20.00000000000000000 ) ;
#13343 = DIRECTION ( 'NONE',  ( -0.4226182617407009401, 0.9063077870366491595, 0.000000000000000000 ) ) ;
#13344 = APPLICATION_PROTOCOL_DEFINITION ( 'draft international standard', 'automotive_design', 1998, #9879 ) ;
#13345 = ORIENTED_EDGE ( 'NONE', *, *, #1444, .F. ) ;
#13346 = CARTESIAN_POINT ( 'NONE',  ( -14.14432607165394629, -111.7272727272741264, 3.395498375151935200 ) ) ;
#13347 = AXIS2_PLACEMENT_3D ( 'NONE', #8738, #13043, #3471 ) ;
#13348 = CARTESIAN_POINT ( 'NONE',  ( -12.99579180576516535, 7.534841976936128560, -1.618136388307047266E-15 ) ) ;
#13349 = CARTESIAN_POINT ( 'NONE',  ( -15.29705854078139993, -19.91286587805129926, -1.803022836769320882E-15 ) ) ;
#13350 = CARTESIAN_POINT ( 'NONE',  ( -10.69346802281034670, -35.22415542633469698, -1.185170506590736236E-15 ) ) ;
#13351 = UNCERTAINTY_MEASURE_WITH_UNIT (LENGTH_MEASURE( 1.000000000000000082E-05 ), #3937, 'distance_accuracy_value', 'NONE');
#13352 = CARTESIAN_POINT ( 'NONE',  ( -14.13596196814457429, -39.17949320881311337, -1.592785305112443692E-15 ) ) ;
#13353 = ADVANCED_FACE ( 'NONE', ( #11608 ), #11807, .T. ) ;
#13354 = AXIS2_PLACEMENT_3D ( 'NONE', #13189, #13269, #7903 ) ;
#13355 = VERTEX_POINT ( 'NONE', #9447 ) ;
#13356 = ORIENTED_EDGE ( 'NONE', *, *, #9951, .T. ) ;
#13357 = ADVANCED_FACE ( 'NONE', ( #11743 ), #7708, .T. ) ;
#13358 = EDGE_LOOP ( 'NONE', ( #315, #460, #4015, #10929 ) ) ;
#13359 = ORIENTED_EDGE ( 'NONE', *, *, #8828, .F. ) ;
#13360 = CARTESIAN_POINT ( 'NONE',  ( 15.29705854078139282, -36.87585420866476937, -30.59411708156276788 ) ) ;
#13361 = CARTESIAN_POINT ( 'NONE',  ( -15.29705854078139282, 90.00000000000000000, -1.589271161308885878E-16 ) ) ;
#13362 = AXIS2_PLACEMENT_3D ( 'NONE', #4939, #10405, #10341 ) ;
#13363 = DIRECTION ( 'NONE',  ( 0.000000000000000000, 0.000000000000000000, 1.000000000000000000 ) ) ;
#13364 = CARTESIAN_POINT ( 'NONE',  ( 1.922734475756564121E-15, -20.00000000000000355, -15.70031846811053455 ) ) ;
#13365 = CARTESIAN_POINT ( 'NONE',  ( -1.861383205662802354, -106.4032560435130534, 6.615796263637743202 ) ) ;
#13366 = CARTESIAN_POINT ( 'NONE',  ( -8.385254915620295790, -6.144721277337255927, 1.085069813372578838E-17 ) ) ;
#13367 = ORIENTED_EDGE ( 'NONE', *, *, #5060, .T. ) ;
#13368 = EDGE_LOOP ( 'NONE', ( #6348, #6573, #9, #7002 ) ) ;
#13369 = ORIENTED_EDGE ( 'NONE', *, *, #2737, .F. ) ;
#13370 = CIRCLE ( 'NONE', #12899, 25.00000000000000711 ) ;
#13371 = ADVANCED_FACE ( 'NONE', ( #6484 ), #10750, .T. ) ;
#13372 = CIRCLE ( 'NONE', #3465, 22.99999999999999289 ) ;
#13373 = ORIENTED_EDGE ( 'NONE', *, *, #8328, .F. ) ;
#13374 = DIRECTION ( 'NONE',  ( 1.000000000000000000, 0.000000000000000000, 0.000000000000000000 ) ) ;
#13375 = CARTESIAN_POINT ( 'NONE',  ( 6.967039245478349407, -74.45454545454340689, 7.244513656184971673 ) ) ;
#13376 = ORIENTED_EDGE ( 'NONE', *, *, #4903, .F. ) ;
#13377 = DIRECTION ( 'NONE',  ( 1.000000000000000000, -0.000000000000000000, -0.000000000000000000 ) ) ;
#13378 = PRODUCT_CONTEXT ( 'NONE', #11576, 'mechanical' ) ;
#13379 = DIRECTION ( 'NONE',  ( -2.797435172181481150E-17, 1.000000000000000000, -1.765856845898762549E-18 ) ) ;
#13380 = CARTESIAN_POINT ( 'NONE',  ( 0.7374174230186665291, -122.9090909090850658, 5.357146445002347157 ) ) ;
#13381 = CARTESIAN_POINT ( 'NONE',  ( 15.29705854078138394, 46.06057977201469100, 30.59411708156277854 ) ) ;
#13382 = DIRECTION ( 'NONE',  ( -0.000000000000000000, -0.000000000000000000, -1.000000000000000000 ) ) ;
#13383 = AXIS2_PLACEMENT_3D ( 'NONE', #9906, #595, #12227 ) ;
#13384 = CARTESIAN_POINT ( 'NONE',  ( -2.401759516268851424, -79.03030303026447712, -10.21173794902991361 ) ) ;
#13385 = CARTESIAN_POINT ( 'NONE',  ( 15.29705854078139282, -1.063309978032472403, 1.873561326908939435E-15 ) ) ;
#13386 = SPHERICAL_SURFACE ( 'NONE', #8683, 5.000000000000000000 ) ;
#13387 = AXIS2_PLACEMENT_3D ( 'NONE', #13148, #3495, #4413 ) ;
#13388 = CARTESIAN_POINT ( 'NONE',  ( 0.000000000000000000, 71.01020514433645303, -2.500000000000000000 ) ) ;
#13389 = CIRCLE ( 'NONE', #4597, 9.000000000008999024 ) ;
#13390 = ORIENTED_EDGE ( 'NONE', *, *, #6341, .F. ) ;
#13391 = DIRECTION ( 'NONE',  ( -0.5999999999999989786, -0.8000000000000008216, 0.000000000000000000 ) ) ;
#13392 = VERTEX_POINT ( 'NONE', #1093 ) ;
#13393 = CARTESIAN_POINT ( 'NONE',  ( 5.805747447557420671, -113.9141079195865842, 1.331989755664621633 ) ) ;
#13394 = AXIS2_PLACEMENT_3D ( 'NONE', #15, #3287, #7431 ) ;
#13395 = DIRECTION ( 'NONE',  ( -0.8000000000000000444, 0.5999999999999999778, 0.000000000000000000 ) ) ;
#13396 = MECHANICAL_DESIGN_GEOMETRIC_PRESENTATION_REPRESENTATION (  '', ( #1702 ), #9761 ) ;
#13397 = DIRECTION ( 'NONE',  ( 0.000000000000000000, 0.000000000000000000, 1.000000000000000000 ) ) ;
#13398 = EDGE_LOOP ( 'NONE', ( #4987, #8761, #8195, #9349, #10166, #10201, #230, #1573, #10174 ) ) ;
#13399 = VERTEX_POINT ( 'NONE', #5354 ) ;
#13400 = CARTESIAN_POINT ( 'NONE',  ( 47.49999999999999289, 120.0000000000000142, 2.499999999999999556 ) ) ;
#13401 = ORIENTED_EDGE ( 'NONE', *, *, #13870, .F. ) ;
#13402 = CARTESIAN_POINT ( 'NONE',  ( 3.426743173711812140, -134.8377289227223628, 0.6876845586499595875 ) ) ;
#13403 = EDGE_CURVE ( 'NONE', #2829, #11706, #11968, .T. ) ;
#13404 = CARTESIAN_POINT ( 'NONE',  ( 0.000000000000000000, -20.00000000000000000, 0.000000000000000000 ) ) ;
#13405 = DIRECTION ( 'NONE',  ( -1.000000000000000000, 0.000000000000000000, 0.000000000000000000 ) ) ;
#13406 = CARTESIAN_POINT ( 'NONE',  ( 155.9864723944028810, -111.6214737678657087, 2.500000000000000000 ) ) ;
#13407 = DIRECTION ( 'NONE',  ( -1.000000000000000000, 0.000000000000000000, 0.000000000000000000 ) ) ;
#13408 = CARTESIAN_POINT ( 'NONE',  ( 35.45454545454547457, 140.4866414850956744, 2.500000000000000000 ) ) ;
#13409 = CARTESIAN_POINT ( 'NONE',  ( -8.385254915620292238, 62.45333659073423860, -1.247464863180835154E-15 ) ) ;
#13410 = DIRECTION ( 'NONE',  ( -0.000000000000000000, -0.000000000000000000, -1.000000000000000000 ) ) ;
#13411 = ORIENTED_EDGE ( 'NONE', *, *, #1987, .T. ) ;
#13412 = CARTESIAN_POINT ( 'NONE',  ( 5.581994045268376503, -105.1818181818169364, -11.80851735648759160 ) ) ;
#13413 = EDGE_LOOP ( 'NONE', ( #7364, #6115, #5112, #11604 ) ) ;
#13414 = CIRCLE ( 'NONE', #3481, 16.99999999999998934 ) ;
#13415 = EDGE_LOOP ( 'NONE', ( #8136, #2296, #741, #13778 ) ) ;
#13416 = LINE ( 'NONE', #8247, #5035 ) ;
#13417 = DIRECTION ( 'NONE',  ( -2.797435172181481150E-17, 1.000000000000000000, -1.765856845898762549E-18 ) ) ;
#13418 = CONTEXT_DEPENDENT_SHAPE_REPRESENTATION ( #3882, #8541 ) ;
#13419 = EDGE_CURVE ( 'NONE', #2480, #7969, #8384, .T. ) ;
#13420 = FACE_OUTER_BOUND ( 'NONE', #9278, .T. ) ;
#13421 = CARTESIAN_POINT ( 'NONE',  ( -8.385254915620292238, 5.904668890677671200, -1.047751159211637166E-15 ) ) ;
#13422 = LINE ( 'NONE', #5885, #7315 ) ;
#13423 = EDGE_CURVE ( 'NONE', #13532, #13094, #3055, .T. ) ;
#13424 = CARTESIAN_POINT ( 'NONE',  ( 12.99553232110414136, 20.49953269456136695, 3.182987412051232168E-15 ) ) ;
#13425 = LINE ( 'NONE', #5956, #7346 ) ;
#13426 = ORIENTED_EDGE ( 'NONE', *, *, #11073, .T. ) ;
#13427 = ORIENTED_EDGE ( 'NONE', *, *, #8176, .T. ) ;
#13428 = CARTESIAN_POINT ( 'NONE',  ( -10.69346802281034137, -25.79937747632526879, -21.38693604562069339 ) ) ;
#13429 = DIRECTION ( 'NONE',  ( -0.9960067511297463483, 0.08927794634716619548, -4.626175998653453504E-17 ) ) ;
#13430 = EDGE_CURVE ( 'NONE', #6441, #8344, #2003, .T. ) ;
#13431 = ORIENTED_EDGE ( 'NONE', *, *, #718, .T. ) ;
#13432 = CARTESIAN_POINT ( 'NONE',  ( 12.99553232110414491, -36.04913500549519512, -25.99106464220827561 ) ) ;
#13433 = CARTESIAN_POINT ( 'NONE',  ( 8.385254915620294014, 78.67828027274755698, 2.053795118489801188E-15 ) ) ;
#13434 = EDGE_CURVE ( 'NONE', #6545, #11738, #10914, .T. ) ;
#13435 = CARTESIAN_POINT ( 'NONE',  ( -2.008006351130390499, -80.00378950643924725, -9.910921267331605833 ) ) ;
#13436 = EDGE_CURVE ( 'NONE', #3703, #4205, #12900, .T. ) ;
#13437 = CARTESIAN_POINT ( 'NONE',  ( -5.411086257474907235, -112.3214038155523298, 2.930518103359322168 ) ) ;
#13438 = CARTESIAN_POINT ( 'NONE',  ( -10.69346802281034492, 49.59884612375012836, -21.38693604562069694 ) ) ;
#13439 = ORIENTED_EDGE ( 'NONE', *, *, #2967, .F. ) ;
#13440 = ORIENTED_EDGE ( 'NONE', *, *, #7382, .F. ) ;
#13441 = CARTESIAN_POINT ( 'NONE',  ( 10.69346802281034847, -6.949821576306441706, 2.619144277183853949E-15 ) ) ;
#13442 = CARTESIAN_POINT ( 'NONE',  ( 8.385254915620294014, 90.00000000000000000, 8.679704431140118580E-16 ) ) ;
#13443 = CIRCLE ( 'NONE', #11818, 2.000000000000003109 ) ;
#13444 = EDGE_CURVE ( 'NONE', #7271, #2160, #6835, .T. ) ;
#13445 = FACE_OUTER_BOUND ( 'NONE', #7283, .T. ) ;
#13446 = ORIENTED_EDGE ( 'NONE', *, *, #11266, .T. ) ;
#13447 = CARTESIAN_POINT ( 'NONE',  ( 7.861734798228629195, -72.85454079061371147, 6.394819286084763910 ) ) ;
#13448 = SURFACE_SIDE_STYLE ('',( #9131 ) ) ;
#13449 = AXIS2_PLACEMENT_3D ( 'NONE', #4002, #788, #10457 ) ;
#13450 = DIRECTION ( 'NONE',  ( 0.000000000000000000, 0.000000000000000000, 1.000000000000000000 ) ) ;
#13451 = CARTESIAN_POINT ( 'NONE',  ( -10.69346802281034137, -16.37459952631584059, -21.38693604562069339 ) ) ;
#13452 = CARTESIAN_POINT ( 'NONE',  ( -0.3134609018057502028, -154.2164502158701964, 0.8036717672344616537 ) ) ;
#13453 = EDGE_CURVE ( 'NONE', #1727, #1229, #11944, .T. ) ;
#13454 = DIRECTION ( 'NONE',  ( -6.158143864569485777E-17, -2.736152283717910599E-16, 1.000000000000000000 ) ) ;
#13455 = CARTESIAN_POINT ( 'NONE',  ( 25.00000000000000355, 120.0000000000000284, 0.5000000000000000000 ) ) ;
#13456 = DIRECTION ( 'NONE',  ( -1.224646799147353207E-16, 1.000000000000000000, -0.000000000000000000 ) ) ;
#13457 = ORIENTED_EDGE ( 'NONE', *, *, #3241, .F. ) ;
#13458 = ORIENTED_EDGE ( 'NONE', *, *, #8833, .F. ) ;
#13459 = CIRCLE ( 'NONE', #4901, 22.49999999999998934 ) ;
#13460 = ORIENTED_EDGE ( 'NONE', *, *, #11809, .F. ) ;
#13461 = LINE ( 'NONE', #535, #2256 ) ;
#13462 = EDGE_CURVE ( 'NONE', #3489, #10825, #8832, .T. ) ;
#13463 = VERTEX_POINT ( 'NONE', #13171 ) ;
#13464 = CARTESIAN_POINT ( 'NONE',  ( 2.124423463547386426, -120.2384439167012005, 4.721629364818086927 ) ) ;
#13465 = DIRECTION ( 'NONE',  ( 1.000000000000000000, 0.000000000000000000, 1.224646799147353207E-16 ) ) ;
#13466 = DIRECTION ( 'NONE',  ( -0.5999999999999999778, -0.8000000000000000444, 0.000000000000000000 ) ) ;
#13467 = DIRECTION ( 'NONE',  ( 0.4545454545454548634, 0.8907235428302464619, 0.000000000000000000 ) ) ;
#13468 = ORIENTED_EDGE ( 'NONE', *, *, #6719, .T. ) ;
#13469 = EDGE_LOOP ( 'NONE', ( #9264, #10390 ) ) ;
#13470 = CARTESIAN_POINT ( 'NONE',  ( 42.49999999999999289, 120.0000000000000142, 2.499999999999999556 ) ) ;
#13471 = CARTESIAN_POINT ( 'NONE',  ( 3.571252647454290496, -130.5986068350643166, -1.733046011458916791 ) ) ;
#13472 = TOROIDAL_SURFACE ( 'NONE', #11849, -34.24999999999974420, 66.24999999999978684 ) ;
#13473 = CARTESIAN_POINT ( 'NONE',  ( 10.00000000000000000, 92.00000000000000000, -2.500000000000000000 ) ) ;
#13474 = LINE ( 'NONE', #7960, #7634 ) ;
#13475 = DIRECTION ( 'NONE',  ( -0.6001121574638170753, 0.7999158696163758409, 1.927470528861191763E-16 ) ) ;
#13476 = CIRCLE ( 'NONE', #7366, 15.29705854078139105 ) ;
#13477 = DIRECTION ( 'NONE',  ( 0.9960067511297463483, -0.08927794634716618161, 4.818676322152979407E-17 ) ) ;
#13478 = DIRECTION ( 'NONE',  ( 1.000000000000000000, 0.000000000000000000, 0.000000000000000000 ) ) ;
#13479 = CARTESIAN_POINT ( 'NONE',  ( 62.16766351966359849, -73.17985663200910551, 2.500000000000000000 ) ) ;
#13480 = ORIENTED_EDGE ( 'NONE', *, *, #13436, .T. ) ;
#13481 = CARTESIAN_POINT ( 'NONE',  ( -8.385254915620292238, 53.02855864072483882, -2.186455329360211015E-15 ) ) ;
#13482 = CIRCLE ( 'NONE', #3124, 8.385254915620290461 ) ;
#13483 = VERTEX_POINT ( 'NONE', #9844 ) ;
#13484 = CARTESIAN_POINT ( 'NONE',  ( -5.849706340270382832, -65.63636363291594478, -2.546235460503720294 ) ) ;
#13485 = VERTEX_POINT ( 'NONE', #12165 ) ;
#13486 = AXIS2_PLACEMENT_3D ( 'NONE', #13239, #9987, #13465 ) ;
#13487 = EDGE_LOOP ( 'NONE', ( #5815, #3520, #12865, #1826 ) ) ;
#13488 = CARTESIAN_POINT ( 'NONE',  ( 8.207015671355002297E-16, -29.33764382806072746, 5.180607919632063331E-17 ) ) ;
#13489 = CARTESIAN_POINT ( 'NONE',  ( -15.68886946032145957, -16.65327071804363612, -0.6902218057983463551 ) ) ;
#13490 = CARTESIAN_POINT ( 'NONE',  ( -10.69381717166375623, 34.98422482212468054, -2.696393829553742293E-15 ) ) ;
#13491 = CIRCLE ( 'NONE', #5837, 5.000000000000000888 ) ;
#13492 = CARTESIAN_POINT ( 'NONE',  ( 55.20422767451771051, -6.230504303137470501, -2.499999999999999112 ) ) ;
#13493 = DIRECTION ( 'NONE',  ( -6.158143864569485777E-17, -2.736152283717910599E-16, 1.000000000000000000 ) ) ;
#13494 = AXIS2_PLACEMENT_3D ( 'NONE', #6403, #4290, #8569 ) ;
#13495 = CARTESIAN_POINT ( 'NONE',  ( 41.99999999999999289, 120.0000000000000142, -0.5000000000000000000 ) ) ;
#13496 = VECTOR ( 'NONE', #8836, 1000.000000000000000 ) ;
#13497 = CARTESIAN_POINT ( 'NONE',  ( -35.20000000000000995, 106.4000000000000199, -0.5000000000000000000 ) ) ;
#13498 = ORIENTED_EDGE ( 'NONE', *, *, #1214, .T. ) ;
#13499 = EDGE_CURVE ( 'NONE', #4205, #9863, #6839, .T. ) ;
#13500 = ORIENTED_EDGE ( 'NONE', *, *, #11820, .T. ) ;
#13501 = CIRCLE ( 'NONE', #4258, 5.000000000000000000 ) ;
#13502 =( BOUNDED_SURFACE ( )  B_SPLINE_SURFACE ( 3, 3, ( 
 ( #11548, #1943, #6290, #3121 ),
 ( #6228, #3977, #12473, #964 ),
 ( #8254, #10492, #12545, #2928 ),
 ( #7200, #5227, #894, #11480 ) ),
 .UNSPECIFIED., .F., .F., .F. ) 
 B_SPLINE_SURFACE_WITH_KNOTS ( ( 4, 4 ),
 ( 4, 4 ),
 ( 0.000000000000000000, 1.000000000000000000 ),
 ( 0.000000000000000000, 1.000000000000000000 ),
 .UNSPECIFIED. ) 
 GEOMETRIC_REPRESENTATION_ITEM ( )  RATIONAL_B_SPLINE_SURFACE ( (
 ( 1.000000000000000000, 0.3333333333333334259, 0.3333333333333334259, 1.000000000000000000),
 ( 1.000000000000000000, 0.3333333333333334259, 0.3333333333333334259, 1.000000000000000000),
 ( 1.000000000000000000, 0.3333333333333334259, 0.3333333333333334259, 1.000000000000000000),
 ( 1.000000000000000000, 0.3333333333333334259, 0.3333333333333334259, 1.000000000000000000) ) ) 
 REPRESENTATION_ITEM ( '' )  SURFACE ( )  );
#13503 = AXIS2_PLACEMENT_3D ( 'NONE', #11381, #9285, #4868 ) ;
#13504 = ORIENTED_EDGE ( 'NONE', *, *, #8325, .T. ) ;
#13505 = CARTESIAN_POINT ( 'NONE',  ( -12.99553232110414136, -36.04913500549519512, -3.146276702057636506E-15 ) ) ;
#13506 = CARTESIAN_POINT ( 'NONE',  ( -12.99553232110414491, 77.04820039461787928, 25.99106464220826851 ) ) ;
#13507 = CARTESIAN_POINT ( 'NONE',  ( 13.79311422413708499, -100.0000000000000000, -7.500000000000000000 ) ) ;
#13508 = DIRECTION ( 'NONE',  ( -1.000000000000000000, 0.000000000000000000, 0.000000000000000000 ) ) ;
#13509 = CARTESIAN_POINT ( 'NONE',  ( 0.6389323985104377046, -103.7399573628443932, 7.199555016268553764 ) ) ;
#13510 = CIRCLE ( 'NONE', #9215, 25.50000000002549783 ) ;
#13511 = CARTESIAN_POINT ( 'NONE',  ( 8.385254915620297567, -31.79444290936001494, -16.77050983124058448 ) ) ;
#13512 = ORIENTED_EDGE ( 'NONE', *, *, #10470, .F. ) ;
#13513 = TOROIDAL_SURFACE ( 'NONE', #3150, 16.99999999999998934, 2.000000000000000000 ) ;
#13514 = EDGE_CURVE ( 'NONE', #5587, #6577, #2727, .T. ) ;
#13515 = AXIS2_PLACEMENT_3D ( 'NONE', #10052, #8934, #8159 ) ;
#13516 = VERTEX_POINT ( 'NONE', #3598 ) ;
#13517 = EDGE_CURVE ( 'NONE', #624, #1587, #1228, .T. ) ;
#13518 = EDGE_CURVE ( 'NONE', #2025, #2515, #6759, .T. ) ;
#13519 = EDGE_CURVE ( 'NONE', #7422, #8450, #10835, .T. ) ;
#13520 = ORIENTED_EDGE ( 'NONE', *, *, #7551, .T. ) ;
#13521 = DIRECTION ( 'NONE',  ( -1.000000000000000000, 0.000000000000000000, 0.000000000000000000 ) ) ;
#13522 = DIRECTION ( 'NONE',  ( 6.158143864569485777E-17, 2.736152283717910599E-16, -1.000000000000000000 ) ) ;
#13523 = EDGE_LOOP ( 'NONE', ( #3476, #11362, #11736, #3478, #3554, #7334, #5187, #5975, #10719, #607, #10499, #8852, #11554 ) ) ;
#13524 = CARTESIAN_POINT ( 'NONE',  ( 9.661733385268016505, -70.21865067213146006, 3.001891211723641373 ) ) ;
#13525 = CIRCLE ( 'NONE', #11454, 18.74900000001875355 ) ;
#13526 = CARTESIAN_POINT ( 'NONE',  ( -12.99579180576516713, 45.23395377697384134, -1.751278857619846450E-15 ) ) ;
#13527 = CARTESIAN_POINT ( 'NONE',  ( 3.039669588831058533, -137.4545454546045846, -0.1626128505627332244 ) ) ;
#13528 = CARTESIAN_POINT ( 'NONE',  ( 28.15981099771517648, -27.70535714287384366, -4.000000000000000000 ) ) ;
#13529 = CARTESIAN_POINT ( 'NONE',  ( -2.517691654963332357E-15, 90.00000000000000000, -1.589271161308885878E-16 ) ) ;
#13530 = ORIENTED_EDGE ( 'NONE', *, *, #7135, .F. ) ;
#13531 = ORIENTED_EDGE ( 'NONE', *, *, #5159, .F. ) ;
#13532 = VERTEX_POINT ( 'NONE', #9778 ) ;
#13533 = CARTESIAN_POINT ( 'NONE',  ( 2.442259928100406263, -119.8068162713657898, 4.626198433201162530 ) ) ;
#13534 = EDGE_CURVE ( 'NONE', #7120, #11569, #12438, .T. ) ;
#13535 = CARTESIAN_POINT ( 'NONE',  ( 15.29705854078138927, 90.00000000000000000, 1.714422261702872766E-15 ) ) ;
#13536 = CARTESIAN_POINT ( 'NONE',  ( -40.81228451836347659, 100.6358150620708471, -0.5000000000000000000 ) ) ;
#13537 = CARTESIAN_POINT ( 'NONE',  ( 18.54049621773915746, 27.07720798312000809, 7.500000000000000000 ) ) ;
#13538 = CARTESIAN_POINT ( 'NONE',  ( -0.1421958018836135540, -122.9182064327156212, -4.881833328960847318 ) ) ;
#13539 = CARTESIAN_POINT ( 'NONE',  ( -0.9182679296299821603, -168.0000000000001421, -0.7188769083877089017 ) ) ;
#13540 = CARTESIAN_POINT ( 'NONE',  ( 10.00000000000000000, 97.99999999999994316, 2.500000000000000000 ) ) ;
#13541 = CYLINDRICAL_SURFACE ( 'NONE', #11630, 10.00000000000000178 ) ;
#13542 = DIRECTION ( 'NONE',  ( 0.000000000000000000, 0.000000000000000000, 1.000000000000000000 ) ) ;
#13543 = DIRECTION ( 'NONE',  ( 0.000000000000000000, 0.000000000000000000, 1.000000000000000000 ) ) ;
#13544 = CARTESIAN_POINT ( 'NONE',  ( -38.16244658108818300, 102.4500712252157797, 2.499999999999999556 ) ) ;
#13545 = DIRECTION ( 'NONE',  ( -1.000000000000000000, 0.000000000000000000, 0.000000000000000000 ) ) ;
#13546 = ORIENTED_EDGE ( 'NONE', *, *, #13218, .T. ) ;
#13547 = AXIS2_PLACEMENT_3D ( 'NONE', #3275, #11828, #8809 ) ;
#13548 = CARTESIAN_POINT ( 'NONE',  ( 15.29705854078138394, 38.52236939141059935, 1.806990092252540040E-15 ) ) ;
#13549 = CARTESIAN_POINT ( 'NONE',  ( -3.794964386186622907, -129.7272727272728901, 2.624161884220013619 ) ) ;
#13550 = CIRCLE ( 'NONE', #1630, 15.29705854078139460 ) ;
#13551 = ADVANCED_FACE ( 'NONE', ( #4733 ), #5707, .T. ) ;
#13552 = ORIENTED_EDGE ( 'NONE', *, *, #2071, .T. ) ;
#13553 = ORIENTED_EDGE ( 'NONE', *, *, #8327, .T. ) ;
#13554 = CARTESIAN_POINT ( 'NONE',  ( -4.895853646792291514, 90.06529264441493865, -1.023585852534433460 ) ) ;
#13555 = DIRECTION ( 'NONE',  ( 0.000000000000000000, 0.000000000000000000, 1.000000000000000000 ) ) ;
#13556 = CARTESIAN_POINT ( 'NONE',  ( 8.385254915620290461, 34.17900274070598243, 9.905219695108648343E-16 ) ) ;
#13557 = DIRECTION ( 'NONE',  ( 0.9960067511297463483, -0.08927794634716618161, 4.818676322152979407E-17 ) ) ;
#13558 = FACE_OUTER_BOUND ( 'NONE', #5733, .T. ) ;
#13559 = CARTESIAN_POINT ( 'NONE',  ( -15.29705854078139105, 19.67281349139177138, -1.942828122597488220E-15 ) ) ;
#13560 = CARTESIAN_POINT ( 'NONE',  ( -2.517691654963332357E-15, 90.00000000000000000, -1.589271161308885878E-16 ) ) ;
#13561 = ORIENTED_EDGE ( 'NONE', *, *, #9201, .F. ) ;
#13562 = AXIS2_PLACEMENT_3D ( 'NONE', #3376, #1157, #5413 ) ;
#13563 = CARTESIAN_POINT ( 'NONE',  ( 42.16244658108818300, 105.4500712252157797, -7.500000000000000000 ) ) ;
#13564 = ORIENTED_EDGE ( 'NONE', *, *, #12697, .T. ) ;
#13565 = CARTESIAN_POINT ( 'NONE',  ( 10.69381717166375800, -21.56444287793185666, 1.362947136962396926E-15 ) ) ;
#13566 = EDGE_CURVE ( 'NONE', #2716, #9777, #407, .T. ) ;
#13567 = CARTESIAN_POINT ( 'NONE',  ( 34.50158885938633802, 107.5319404580926630, 2.003700325319508035 ) ) ;
#13568 = AXIS2_PLACEMENT_3D ( 'NONE', #7935, #587, #9127 ) ;
#13569 = CARTESIAN_POINT ( 'NONE',  ( -8.385254915620288685, -3.520109059331755663, -16.77050983124058448 ) ) ;
#13570 = DIRECTION ( 'NONE',  ( 0.000000000000000000, 0.000000000000000000, -1.000000000000000000 ) ) ;
#13571 = CARTESIAN_POINT ( 'NONE',  ( 8.320762423101355054, -90.25487416876752889, -3.125163722747064110 ) ) ;
#13572 = LINE ( 'NONE', #2874, #864 ) ;
#13573 = ORIENTED_EDGE ( 'NONE', *, *, #6356, .F. ) ;
#13574 = EDGE_LOOP ( 'NONE', ( #10132, #1676, #395, #12120 ) ) ;
#13575 = VECTOR ( 'NONE', #5580, 1000.000000000000000 ) ;
#13576 = CIRCLE ( 'NONE', #2334, 8.385254915620294014 ) ;
#13577 = ORIENTED_EDGE ( 'NONE', *, *, #3110, .F. ) ;
#13578 = CARTESIAN_POINT ( 'NONE',  ( 1.387778780781445676E-14, -135.0000000000000000, 0.000000000000000000 ) ) ;
#13579 = CYLINDRICAL_SURFACE ( 'NONE', #2228, 24.99999999999998934 ) ;
#13580 = AXIS2_PLACEMENT_3D ( 'NONE', #8045, #12327, #6994 ) ;
#13581 = VERTEX_POINT ( 'NONE', #4507 ) ;
#13582 = LINE ( 'NONE', #3024, #11497 ) ;
#13583 = EDGE_CURVE ( 'NONE', #1929, #7574, #3688, .T. ) ;
#13584 = DIRECTION ( 'NONE',  ( -6.158143864569485777E-17, -2.736152283717910599E-16, 1.000000000000000000 ) ) ;
#13585 = ADVANCED_FACE ( 'NONE', ( #1500 ), #9918, .F. ) ;
#13586 = DIRECTION ( 'NONE',  ( -1.000000000000000000, 0.000000000000000000, 0.000000000000000000 ) ) ;
#13587 = DIRECTION ( 'NONE',  ( 1.000000000000000000, 0.000000000000000000, 0.000000000000000000 ) ) ;
#13588 = CARTESIAN_POINT ( 'NONE',  ( -2.035923840464202161, -145.3956134166558058, -1.226378594624949026 ) ) ;
#13589 = EDGE_CURVE ( 'NONE', #12324, #2480, #7054, .T. ) ;
#13590 = PLANE ( 'NONE',  #10855 ) ;
#13591 = AXIS2_PLACEMENT_3D ( 'NONE', #232, #1270, #5474 ) ;
#13592 = EDGE_CURVE ( 'NONE', #3902, #2799, #12016, .T. ) ;
#13593 = ORIENTED_EDGE ( 'NONE', *, *, #1283, .T. ) ;
#13594 = ORIENTED_EDGE ( 'NONE', *, *, #13689, .T. ) ;
#13595 = AXIS2_PLACEMENT_3D ( 'NONE', #9222, #3747, #9084 ) ;
#13596 = ORIENTED_EDGE ( 'NONE', *, *, #2561, .F. ) ;
#13597 = CARTESIAN_POINT ( 'NONE',  ( 5.850599514082611030, -109.0563038876532573, -2.972233473650054858 ) ) ;
#13598 = DIRECTION ( 'NONE',  ( -1.000000000000000000, 0.000000000000000000, 0.000000000000000000 ) ) ;
#13599 = DIRECTION ( 'NONE',  ( -1.000000000000000000, 0.000000000000000000, 0.000000000000000000 ) ) ;
#13600 = AXIS2_PLACEMENT_3D ( 'NONE', #310, #529, #1487 ) ;
#13601 = CARTESIAN_POINT ( 'NONE',  ( -35.00000000000000000, -4.286263797015736496E-15, 10.49999999999999822 ) ) ;
#13602 = CARTESIAN_POINT ( 'NONE',  ( -1.135377999189010501, -155.8397449083613822, -1.102628456091256703 ) ) ;
#13603 = EDGE_CURVE ( 'NONE', #10943, #7680, #11755, .T. ) ;
#13604 = CARTESIAN_POINT ( 'NONE',  ( -0.5095487865723351550, -163.8787878240969746, -3.239446892380866583 ) ) ;
#13605 = DIRECTION ( 'NONE',  ( 0.4206864060305147146, -0.9072061219927525233, -2.409338161076489703E-16 ) ) ;
#13606 =( GEOMETRIC_REPRESENTATION_CONTEXT ( 3 ) GLOBAL_UNCERTAINTY_ASSIGNED_CONTEXT ( ( #13046 ) ) GLOBAL_UNIT_ASSIGNED_CONTEXT ( ( #12427, #11164, #10039 ) ) REPRESENTATION_CONTEXT ( 'NONE', 'WORKASPACE' ) );
#13607 = ADVANCED_FACE ( 'NONE', ( #12386 ), #9965, .T. ) ;
#13608 = CARTESIAN_POINT ( 'NONE',  ( 15.29705854078138927, 19.67281349139177138, 1.840275709580740132E-15 ) ) ;
#13609 = AXIS2_PLACEMENT_3D ( 'NONE', #3222, #7500, #4204 ) ;
#13610 = DIRECTION ( 'NONE',  ( 0.000000000000000000, 0.000000000000000000, -1.000000000000000000 ) ) ;
#13611 = CARTESIAN_POINT ( 'NONE',  ( 55.00383357371546822, 6.846651893462918359, 2.500000000000003109 ) ) ;
#13612 = EDGE_CURVE ( 'NONE', #3335, #6530, #2773, .T. ) ;
#13613 = DIRECTION ( 'NONE',  ( -0.000000000000000000, -0.000000000000000000, -1.000000000000000000 ) ) ;
#13614 = EDGE_CURVE ( 'NONE', #8762, #1146, #4824, .T. ) ;
#13615 = AXIS2_PLACEMENT_3D ( 'NONE', #11981, #10100, #9957 ) ;
#13616 = CARTESIAN_POINT ( 'NONE',  ( 10.00000000000000711, 139.9999999999999716, 0.5000000000000000000 ) ) ;
#13617 = ORIENTED_EDGE ( 'NONE', *, *, #5963, .T. ) ;
#13618 = DIRECTION ( 'NONE',  ( 1.000000000000000000, 0.000000000000000000, 0.000000000000000000 ) ) ;
#13619 = AXIS2_PLACEMENT_3D ( 'NONE', #2147, #4247, #7541 ) ;
#13620 = CARTESIAN_POINT ( 'NONE',  ( 6.295302227001586814, -164.3636363559542701, -1.035156591622384159 ) ) ;
#13621 = AXIS2_PLACEMENT_3D ( 'NONE', #12666, #5142, #9431 ) ;
#13622 = ORIENTED_EDGE ( 'NONE', *, *, #10066, .F. ) ;
#13623 = ORIENTED_EDGE ( 'NONE', *, *, #12917, .T. ) ;
#13624 = DIRECTION ( 'NONE',  ( 5.551115123125776539E-17, -1.000000000000000000, -3.204747427460360459E-31 ) ) ;
#13625 = DIRECTION ( 'NONE',  ( 0.000000000000000000, 0.000000000000000000, -1.000000000000000000 ) ) ;
#13626 = EDGE_CURVE ( 'NONE', #3469, #9005, #1453, .T. ) ;
#13627 = AXIS2_PLACEMENT_3D ( 'NONE', #4975, #9254, #13570 ) ;
#13628 = CARTESIAN_POINT ( 'NONE',  ( 15.29705854078139282, -8.601520358636511432, 1.890204135573039875E-15 ) ) ;
#13629 = LINE ( 'NONE', #1874, #10007 ) ;
#13630 = EDGE_CURVE ( 'NONE', #4098, #12961, #9304, .T. ) ;
#13631 = DIRECTION ( 'NONE',  ( -0.000000000000000000, -0.000000000000000000, -1.000000000000000000 ) ) ;
#13632 = CARTESIAN_POINT ( 'NONE',  ( -29.00000000000000000, 123.0000000000000142, 7.500000000000000000 ) ) ;
#13633 = CIRCLE ( 'NONE', #9338, 25.00000000000000355 ) ;
#13634 = ORIENTED_EDGE ( 'NONE', *, *, #4816, .T. ) ;
#13635 = EDGE_LOOP ( 'NONE', ( #12265, #6757, #5268, #3078 ) ) ;
#13636 = EDGE_LOOP ( 'NONE', ( #12831, #2393, #3738, #9910 ) ) ;
#13637 = CARTESIAN_POINT ( 'NONE',  ( 80.29381926039658879, -64.72749139719506672, 2.500000000000000000 ) ) ;
#13638 = CARTESIAN_POINT ( 'NONE',  ( 52.82363224725100537, -5.817485239812894449, 2.500000000000000000 ) ) ;
#13639 = CARTESIAN_POINT ( 'NONE',  ( 34.58461996471805122, 107.3565440455617477, 2.151643583074652977 ) ) ;
#13640 = FACE_OUTER_BOUND ( 'NONE', #6962, .T. ) ;
#13641 = CARTESIAN_POINT ( 'NONE',  ( -34.58386302044580418, 107.3580618547655803, 2.150514425741564484 ) ) ;
#13642 = CARTESIAN_POINT ( 'NONE',  ( 2.981500127671308675, -138.8769926725574635, -0.6020624928271046672 ) ) ;
#13643 = FACE_OUTER_BOUND ( 'NONE', #9909, .T. ) ;
#13644 = ORIENTED_EDGE ( 'NONE', *, *, #2065, .F. ) ;
#13645 = ORIENTED_EDGE ( 'NONE', *, *, #10963, .T. ) ;
#13646 = VERTEX_POINT ( 'NONE', #13537 ) ;
#13647 = VERTEX_POINT ( 'NONE', #4806 ) ;
#13648 = FACE_OUTER_BOUND ( 'NONE', #427, .T. ) ;
#13649 = ORIENTED_EDGE ( 'NONE', *, *, #6433, .F. ) ;
#13650 = CARTESIAN_POINT ( 'NONE',  ( 9.637068721888157441, -69.33333333333251858, 3.199157287630882252 ) ) ;
#13651 = ORIENTED_EDGE ( 'NONE', *, *, #7288, .T. ) ;
#13652 = DIRECTION ( 'NONE',  ( -1.000000000000000000, 0.000000000000000000, 0.000000000000000000 ) ) ;
#13653 = CARTESIAN_POINT ( 'NONE',  ( -4.278103086406176203, -97.41991341992381592, -7.774081346650261182 ) ) ;
#13654 = DIRECTION ( 'NONE',  ( -2.797435172181481150E-17, 1.000000000000000000, -1.765856845898762549E-18 ) ) ;
#13655 = CARTESIAN_POINT ( 'NONE',  ( -15.69972745459287822, -22.78055882083340222, -0.6693078754302107525 ) ) ;
#13656 = FACE_OUTER_BOUND ( 'NONE', #10296, .T. ) ;
#13657 = CARTESIAN_POINT ( 'NONE',  ( 3.202161775521378484, -122.5503334129114279, 3.775223943724925313 ) ) ;
#13658 = CARTESIAN_POINT ( 'NONE',  ( 32.50998312217522113, 0.2231948658680255881, -2.499999999999997335 ) ) ;
#13659 = ORIENTED_EDGE ( 'NONE', *, *, #7123, .T. ) ;
#13660 = DIRECTION ( 'NONE',  ( -2.797435172181481150E-17, 1.000000000000000000, -1.765856845898762549E-18 ) ) ;
#13661 = ORIENTED_EDGE ( 'NONE', *, *, #8308, .T. ) ;
#13662 = ADVANCED_FACE ( 'NONE', ( #2836 ), #8181, .F. ) ;
#13663 = CIRCLE ( 'NONE', #12049, 2.000000000000001776 ) ;
#13664 = EDGE_CURVE ( 'NONE', #12240, #3719, #9075, .T. ) ;
#13665 = CIRCLE ( 'NONE', #7780, 2.000000000000000000 ) ;
#13666 = DIRECTION ( 'NONE',  ( -0.000000000000000000, -0.000000000000000000, -1.000000000000000000 ) ) ;
#13667 = PRODUCT_RELATED_PRODUCT_CATEGORY ( 'part', '', ( #1387 ) ) ;
#13668 = EDGE_LOOP ( 'NONE', ( #10030, #11171, #8244, #5596 ) ) ;
#13669 = CARTESIAN_POINT ( 'NONE',  ( -15.29705854078138749, 38.52236939141059935, -3.816389449506426866E-15 ) ) ;
#13670 = CARTESIAN_POINT ( 'NONE',  ( 8.869476657224877769, -90.43147964619883794, 0.05619714888382777024 ) ) ;
#13671 = CARTESIAN_POINT ( 'NONE',  ( -0.2677229415630820730, -160.9696969673928209, 0.7106593571390205089 ) ) ;
#13672 = CARTESIAN_POINT ( 'NONE',  ( 48.00000000000000000, 120.0000000000000142, 0.5000000000000000000 ) ) ;
#13673 = DIRECTION ( 'NONE',  ( -0.000000000000000000, -0.000000000000000000, -1.000000000000000000 ) ) ;
#13674 = DIRECTION ( 'NONE',  ( 1.000000000000000000, 0.000000000000000000, 0.000000000000000000 ) ) ;
#13675 = B_SPLINE_CURVE_WITH_KNOTS ( 'NONE', 3,
 ( #7061, #4604, #10085, #422, #3621, #8887, #4679, #3695, #5657, #7983, #499, #8048, #3840, #9168, #2794, #2508 ),
 .UNSPECIFIED., .F., .F.,
 ( 4, 2, 2, 2, 2, 2, 2, 4 ),
 ( 0.001123485749927461298, 0.001530777205506884606, 0.001938068661086307914, 0.002345360116665731222, 0.002752651572245154964, 0.003159943027824578272, 0.003567234483404001580, 0.004381817394562857737 ),
 .UNSPECIFIED. ) ;
#13676 = DIRECTION ( 'NONE',  ( 0.000000000000000000, 0.000000000000000000, 1.000000000000000000 ) ) ;
#13677 = DIRECTION ( 'NONE',  ( 1.000000000000000000, 0.000000000000000000, 0.000000000000000000 ) ) ;
#13678 = AXIS2_PLACEMENT_3D ( 'NONE', #9544, #13726, #7428 ) ;
#13679 = DIRECTION ( 'NONE',  ( 1.000000000000000000, 0.000000000000000000, 0.000000000000000000 ) ) ;
#13680 = ADVANCED_FACE ( 'NONE', ( #1572 ), #3239, .T. ) ;
#13681 = ORIENTED_EDGE ( 'NONE', *, *, #12641, .F. ) ;
#13682 = DIRECTION ( 'NONE',  ( 0.000000000000000000, 1.000000000000000000, 0.000000000000000000 ) ) ;
#13683 = CARTESIAN_POINT ( 'NONE',  ( 3.361332843921851943, -147.1038961038433968, 14.17852599539457259 ) ) ;
#13684 = ADVANCED_FACE ( 'NONE', ( #12241 ), #669, .T. ) ;
#13685 = VERTEX_POINT ( 'NONE', #8103 ) ;
#13686 = B_SPLINE_CURVE_WITH_KNOTS ( 'NONE', 3,
 ( #1716, #9287, #3888, #546, #4871, #2632, #10342, #12387, #13602, #13322, #6978, #6898, #12518, #471, #11187, #7109, #743, #11458, #2902, #3673, #4808, #10060, #10203, #5008, #5864, #9015, #7957, #9086, #10137, #9149, #13402, #2703, #11259, #1649, #5932, #2774, #13471, #3816, #8104, #7041, #6002, #10267, #670, #4940, #9223, #13538, #8167, #7441, #10668, #8498, #3232, #2054, #7511, #1849, #11659, #6331, #1983, #7371, #11723, #5205, #12725, #12868, #4083, #6136, #4017, #10406, #10603, #6264, #9560, #2113, #6400, #9493, #9358, #1006, #4152, #942, #10467, #13740, #807, #10535, #6207, #1076, #870, #7242, #3041, #8564, #13802, #5275, #3166, #5077, #13869, #8436, #13670, #4216, #8367, #5340, #12794, #9624, #32, #5138, #3101, #4285, #9426, #8300, #12594, #2973, #11525, #1918, #12660, #7310, #11594, #1149, #11857, #3298 ),
 .UNSPECIFIED., .F., .F.,
 ( 4, 2, 2, 2, 2, 2, 2, 2, 2, 2, 2, 2, 2, 2, 2, 2, 2, 2, 2, 2, 2, 2, 2, 2, 2, 2, 2, 2, 2, 2, 2, 2, 2, 2, 2, 2, 2, 2, 2, 2, 2, 2, 2, 2, 2, 2, 2, 2, 2, 2, 2, 2, 2, 2, 2, 2, 4 ),
 ( 2.168404344971008868E-19, 0.0008229045663924312816, 0.001645809132784862346, 0.003291618265569724693, 0.004937427398354586605, 0.006583236531139448518, 0.009874854796709173210, 0.01152066392949403426, 0.01316647306227889704, 0.01481228219506375982, 0.01645809132784862086, 0.01974970959341826662, 0.02139551872620305134, 0.02304132785898783606, 0.02633294612455740549, 0.02797875525734215552, 0.02962456439012690901, 0.03127037352291166250, 0.03291618265569640905, 0.03620780092126597849, 0.03785361005405073198, 0.03949941918683547853, 0.04114522831962022509, 0.04279103745240498552, 0.04608265571797444393, 0.04772846485075918355, 0.04937427398354391622, 0.05102008311632864890, 0.05184298768272101871, 0.05266589224911337463, 0.05595751051468290937, 0.05924912878025244412, 0.06089493791303720455, 0.06254074704582197886, 0.06418655617860674623, 0.06583236531139149972, 0.06912398357696107609, 0.07076979270974584346, 0.07241560184253061083, 0.07406141097531537820, 0.07570722010810014557, 0.07899883837366970807, 0.08064464750645450319, 0.08229045663923928444, 0.08393626577202409345, 0.08558207490480887469, 0.08887369317037849270, 0.09051950230316328783, 0.09216531143594809683, 0.09381112056873290583, 0.09545692970151771484, 0.09710273883430250996, 0.09874854796708731897, 0.1020401662326569370, 0.1036859753654417460, 0.1045088799318341505, 0.1053317844982265411 ),
 .UNSPECIFIED. ) ;
#13687 = CYLINDRICAL_SURFACE ( 'NONE', #4576, 8.385254915620292238 ) ;
#13688 = AXIS2_PLACEMENT_3D ( 'NONE', #10864, #1151, #11996 ) ;
#13689 = EDGE_CURVE ( 'NONE', #1355, #6722, #8611, .T. ) ;
#13690 = ORIENTED_EDGE ( 'NONE', *, *, #12128, .T. ) ;
#13691 = CARTESIAN_POINT ( 'NONE',  ( -9.637068721888248035, -69.33333333333280279, -3.199157287630891133 ) ) ;
#13692 = ADVANCED_FACE ( 'NONE', ( #9286 ), #1647, .T. ) ;
#13693 = DIRECTION ( 'NONE',  ( -2.797435172181481150E-17, 1.000000000000000000, -1.765856845898762549E-18 ) ) ;
#13694 = TOROIDAL_SURFACE ( 'NONE', #3791, 16.99999999999998934, 2.000000000000000000 ) ;
#13695 = CARTESIAN_POINT ( 'NONE',  ( 5.912741558351815918, -73.45454546935906137, 18.82838426099241858 ) ) ;
#13696 = CARTESIAN_POINT ( 'NONE',  ( 19.28867028138563811, -167.3636363504097346, -6.559046149895597644 ) ) ;
#13697 = CARTESIAN_POINT ( 'NONE',  ( 82.09155748149851206, -71.43674177705591433, 2.500000000000000000 ) ) ;
#13698 = CARTESIAN_POINT ( 'NONE',  ( -8.385254915620292238, -22.36966495935058319, -9.478943072270380731E-16 ) ) ;
#13699 = DIRECTION ( 'NONE',  ( -2.797435172181481150E-17, 1.000000000000000000, -1.765856845898762549E-18 ) ) ;
#13700 = VECTOR ( 'NONE', #11927, 1000.000000000000000 ) ;
#13701 = CARTESIAN_POINT ( 'NONE',  ( 0.6173387890061948768, -70.00000000000000000, -4.961742921553712549 ) ) ;
#13702 = AXIS2_PLACEMENT_3D ( 'NONE', #1019, #10549, #2914 ) ;
#13703 = ORIENTED_EDGE ( 'NONE', *, *, #9527, .F. ) ;
#13704 = EDGE_CURVE ( 'NONE', #1407, #7751, #2901, .T. ) ;
#13705 = AXIS2_PLACEMENT_3D ( 'NONE', #747, #11118, #3603 ) ;
#13706 = ORIENTED_EDGE ( 'NONE', *, *, #2999, .F. ) ;
#13707 = CARTESIAN_POINT ( 'NONE',  ( 53.56517978609545594, 2.618988451796029349, -2.499999999999997335 ) ) ;
#13708 = CARTESIAN_POINT ( 'NONE',  ( -35.45454545454546036, 140.4866414850956744, 2.500000000000000000 ) ) ;
#13709 = CIRCLE ( 'NONE', #9656, 20.00000000000001066 ) ;
#13710 = VECTOR ( 'NONE', #4264, 1000.000000000000000 ) ;
#13711 = FACE_OUTER_BOUND ( 'NONE', #11868, .T. ) ;
#13712 = LINE ( 'NONE', #10503, #10102 ) ;
#13713 = CARTESIAN_POINT ( 'NONE',  ( 0.03718945268892032141, -157.3606764272614669, 1.516196336863006477 ) ) ;
#13714 = DIRECTION ( 'NONE',  ( -1.000000000000000000, 0.000000000000000000, 0.000000000000000000 ) ) ;
#13715 = VECTOR ( 'NONE', #6052, 1000.000000000000000 ) ;
#13716 = ORIENTED_EDGE ( 'NONE', *, *, #1503, .F. ) ;
#13717 = AXIS2_PLACEMENT_3D ( 'NONE', #3120, #8522, #1873 ) ;
#13718 = CIRCLE ( 'NONE', #5167, 9.000000000008999024 ) ;
#13719 = VERTEX_POINT ( 'NONE', #11457 ) ;
#13720 = CYLINDRICAL_SURFACE ( 'NONE', #13798, 2.000000000000001776 ) ;
#13721 = ORIENTED_EDGE ( 'NONE', *, *, #13765, .F. ) ;
#13722 = CARTESIAN_POINT ( 'NONE',  ( 15.29705854078139282, -38.76242177807012723, 1.940132561565339619E-15 ) ) ;
#13723 = ORIENTED_EDGE ( 'NONE', *, *, #8748, .F. ) ;
#13724 = DIRECTION ( 'NONE',  ( -6.158143864569485777E-17, -2.736152283717910599E-16, 1.000000000000000000 ) ) ;
#13725 = AXIS2_PLACEMENT_3D ( 'NONE', #11192, #7048, #4876 ) ;
#13726 = DIRECTION ( 'NONE',  ( 0.000000000000000000, 0.000000000000000000, 1.000000000000000000 ) ) ;
#13727 = CARTESIAN_POINT ( 'NONE',  ( 25.00000000000000355, 120.0000000000000142, -2.499999999999998668 ) ) ;
#13728 = CYLINDRICAL_SURFACE ( 'NONE', #13135, 2.500000000000002220 ) ;
#13729 = AXIS2_PLACEMENT_3D ( 'NONE', #4751, #3613, #2785 ) ;
#13730 = CARTESIAN_POINT ( 'NONE',  ( -0.3891315833696432636, -154.2086256632273944, -1.618697729122736018 ) ) ;
#13731 = CYLINDRICAL_SURFACE ( 'NONE', #5967, 25.50000000002549783 ) ;
#13732 = ORIENTED_EDGE ( 'NONE', *, *, #10660, .F. ) ;
#13733 = ORIENTED_EDGE ( 'NONE', *, *, #7997, .T. ) ;
#13734 = ORIENTED_EDGE ( 'NONE', *, *, #2309, .F. ) ;
#13735 = DIRECTION ( 'NONE',  ( 1.077462011625539371E-16, -1.454589777793963520E-16, 1.000000000000000000 ) ) ;
#13736 = AXIS2_PLACEMENT_3D ( 'NONE', #1920, #12596, #4085 ) ;
#13737 = CARTESIAN_POINT ( 'NONE',  ( -12.99553232110413781, 39.34908859458022334, -1.730463420974848368E-15 ) ) ;
#13738 = CARTESIAN_POINT ( 'NONE',  ( 1.236368069360658017, -80.00117829049393947, 9.950313871619497874 ) ) ;
#13739 = DIRECTION ( 'NONE',  ( -0.000000000000000000, -0.000000000000000000, -1.000000000000000000 ) ) ;
#13740 = CARTESIAN_POINT ( 'NONE',  ( 1.581460637658297141, -99.95560608173282446, 7.500979497773645477 ) ) ;
#13741 = CARTESIAN_POINT ( 'NONE',  ( -15.29705854078139637, 64.91013567203349055, -3.859655058983359639E-15 ) ) ;
#13742 = FACE_OUTER_BOUND ( 'NONE', #1964, .T. ) ;
#13743 = CARTESIAN_POINT ( 'NONE',  ( 10.69346802281034847, 2.474956373702985601, 1.309720302413869460E-15 ) ) ;
#13744 = DIRECTION ( 'NONE',  ( -6.158143864569485777E-17, -2.736152283717910599E-16, 1.000000000000000000 ) ) ;
#13745 = DIRECTION ( 'NONE',  ( -6.158143864569485777E-17, -2.736152283717910599E-16, 1.000000000000000000 ) ) ;
#13746 = AXIS2_PLACEMENT_3D ( 'NONE', #4563, #13382, #3732 ) ;
#13747 = ORIENTED_EDGE ( 'NONE', *, *, #11002, .F. ) ;
#13748 = FACE_OUTER_BOUND ( 'NONE', #1999, .T. ) ;
#13749 = DIRECTION ( 'NONE',  ( 1.000000000000000000, 0.000000000000000000, 0.000000000000000000 ) ) ;
#13750 = CARTESIAN_POINT ( 'NONE',  ( -1.916816365364703234, -124.8181818181863747, -4.196942880910714990 ) ) ;
#13751 = VERTEX_POINT ( 'NONE', #6135 ) ;
#13752 = CARTESIAN_POINT ( 'NONE',  ( 15.18222645069203303, 20.00000000000000000, -4.000000000000000000 ) ) ;
#13753 = ORIENTED_EDGE ( 'NONE', *, *, #8067, .T. ) ;
#13754 = CARTESIAN_POINT ( 'NONE',  ( 25.00000000000000355, 120.0000000000000142, 2.499999999999999556 ) ) ;
#13755 = FACE_OUTER_BOUND ( 'NONE', #11267, .T. ) ;
#13756 = CARTESIAN_POINT ( 'NONE',  ( 14.37641089434894326, -21.93614314624078787, -6.343488216808988334 ) ) ;
#13757 = CARTESIAN_POINT ( 'NONE',  ( -6.075667645225103719, -100.2727272727262147, -11.56208117637899058 ) ) ;
#13758 = EDGE_CURVE ( 'NONE', #11837, #11393, #6591, .T. ) ;
#13759 = DIRECTION ( 'NONE',  ( -6.158143864569485777E-17, -2.736152283717910599E-16, 1.000000000000000000 ) ) ;
#13760 = EDGE_CURVE ( 'NONE', #2956, #11003, #8395, .T. ) ;
#13761 = EDGE_CURVE ( 'NONE', #3156, #13094, #4133, .T. ) ;
#13762 = CARTESIAN_POINT ( 'NONE',  ( 35.20000000000001705, 106.4000000000000199, -0.5000000000000000000 ) ) ;
#13763 = CYLINDRICAL_SURFACE ( 'NONE', #12299, 80.00000000000001421 ) ;
#13764 = EDGE_CURVE ( 'NONE', #9113, #11308, #6394, .T. ) ;
#13765 = EDGE_CURVE ( 'NONE', #2392, #6130, #11258, .T. ) ;
#13766 = ORIENTED_EDGE ( 'NONE', *, *, #9271, .T. ) ;
#13767 =( REPRESENTATION_RELATIONSHIP ('NONE','NONE', #9450, #12318 ) REPRESENTATION_RELATIONSHIP_WITH_TRANSFORMATION ( #11132 )SHAPE_REPRESENTATION_RELATIONSHIP( ) );
#13768 = AXIS2_PLACEMENT_3D ( 'NONE', #11550, #7331, #5230 ) ;
#13769 = CIRCLE ( 'NONE', #1645, 9.000000000009002576 ) ;
#13770 = DIRECTION ( 'NONE',  ( 6.158143864569485777E-17, 2.736152283717910599E-16, -1.000000000000000000 ) ) ;
#13771 = CARTESIAN_POINT ( 'NONE',  ( -21.99999999999999289, -97.00000000000000000, 7.500000000000000000 ) ) ;
#13772 = CARTESIAN_POINT ( 'NONE',  ( 34.46489414126431683, 107.6161901685304372, 1.920132901535068326 ) ) ;
#13773 = EDGE_CURVE ( 'NONE', #1244, #10453, #3249, .T. ) ;
#13774 = DIRECTION ( 'NONE',  ( -1.000000000000000000, 0.000000000000000000, 0.000000000000000000 ) ) ;
#13775 = DIRECTION ( 'NONE',  ( 0.000000000000000000, 0.000000000000000000, 1.000000000000000000 ) ) ;
#13776 = CARTESIAN_POINT ( 'NONE',  ( 13.79311422413708499, -21.62638421600850691, 7.500000000000000000 ) ) ;
#13777 = ADVANCED_FACE ( 'NONE', ( #8366 ), #7440, .T. ) ;
#13778 = ORIENTED_EDGE ( 'NONE', *, *, #7707, .F. ) ;
#13779 = VERTEX_POINT ( 'NONE', #2180 ) ;
#13780 = CARTESIAN_POINT ( 'NONE',  ( -2.179449471770338320, 90.00000000000000000, -4.500000000000000888 ) ) ;
#13781 = ORIENTED_EDGE ( 'NONE', *, *, #3614, .F. ) ;
#13782 = DIRECTION ( 'NONE',  ( -1.000000000000000000, 0.000000000000000000, 0.000000000000000000 ) ) ;
#13783 = CARTESIAN_POINT ( 'NONE',  ( 0.000000000000000000, 71.01020514433645303, 2.499999999999999556 ) ) ;
#13784 = ORIENTED_EDGE ( 'NONE', *, *, #6628, .F. ) ;
#13785 = CARTESIAN_POINT ( 'NONE',  ( 10.69381717166375623, 6.709890972096427042, 0.000000000000000000 ) ) ;
#13786 = TOROIDAL_SURFACE ( 'NONE', #10169, 3.999999999999998224, 2.000000000000000000 ) ;
#13787 = CARTESIAN_POINT ( 'NONE',  ( 82.09155748149851206, -71.43674177705591433, -2.500000000000000000 ) ) ;
#13788 = CARTESIAN_POINT ( 'NONE',  ( -15.37190086779363263, -22.55217709030015527, 3.259922557882396710 ) ) ;
#13789 = CARTESIAN_POINT ( 'NONE',  ( -2.517691654963332357E-15, 90.00000000000000000, -1.589271161308885878E-16 ) ) ;
#13790 = CARTESIAN_POINT ( 'NONE',  ( -8.385254915620295790, 69.25350232273815720, -2.234634242108977241E-15 ) ) ;
#13791 = CARTESIAN_POINT ( 'NONE',  ( 0.8868958219609875959, -105.3243828844967851, -6.976889881733200127 ) ) ;
#13792 = CARTESIAN_POINT ( 'NONE',  ( -25.00000000000000355, 120.0000000000000284, 2.500000000000000000 ) ) ;
#13793 = EDGE_LOOP ( 'NONE', ( #1454, #2404, #1825, #10742 ) ) ;
#13794 = EDGE_CURVE ( 'NONE', #8040, #6479, #6848, .T. ) ;
#13795 = ORIENTED_EDGE ( 'NONE', *, *, #5666, .F. ) ;
#13796 = DIRECTION ( 'NONE',  ( -1.000000000000000000, 0.000000000000000000, 0.000000000000000000 ) ) ;
#13797 = ORIENTED_EDGE ( 'NONE', *, *, #7609, .F. ) ;
#13798 = AXIS2_PLACEMENT_3D ( 'NONE', #3018, #4065, #11570 ) ;
#13799 = DIRECTION ( 'NONE',  ( -1.224646799147353207E-16, 1.000000000000000000, -0.000000000000000000 ) ) ;
#13800 = VERTEX_POINT ( 'NONE', #10534 ) ;
#13801 = DIRECTION ( 'NONE',  ( -1.000000000000000000, 0.000000000000000000, 0.000000000000000000 ) ) ;
#13802 = CARTESIAN_POINT ( 'NONE',  ( 7.157689724239170381, -94.21585681134573065, 4.329420255253605632 ) ) ;
#13803 = CIRCLE ( 'NONE', #9068, 2.500000000000002220 ) ;
#13804 = DIRECTION ( 'NONE',  ( 6.158143864569485777E-17, 2.736152283717910599E-16, -1.000000000000000000 ) ) ;
#13805 = CARTESIAN_POINT ( 'NONE',  ( -10.69381717166375090, 63.25855867215300066, -21.38763434332750890 ) ) ;
#13806 = AXIS2_PLACEMENT_3D ( 'NONE', #12740, #5221, #4168 ) ;
#13807 = CARTESIAN_POINT ( 'NONE',  ( -12.99553232110414314, 20.49953269456136695, -3.227288338581441853E-15 ) ) ;
#13808 = CARTESIAN_POINT ( 'NONE',  ( -8.385254915620294014, 3.280056672672170937, -2.065495521823092020E-15 ) ) ;
#13809 = AXIS2_PLACEMENT_3D ( 'NONE', #4102, #6418, #11675 ) ;
#13810 = DIRECTION ( 'NONE',  ( -0.8735848310779960046, 0.4866719047884613403, 6.939263997980181797E-17 ) ) ;
#13811 = DIRECTION ( 'NONE',  ( 1.000000000000000000, 0.000000000000000000, 0.000000000000000000 ) ) ;
#13812 = LINE ( 'NONE', #9502, #9181 ) ;
#13813 = CARTESIAN_POINT ( 'NONE',  ( 12.65441377644658338, -89.44155844155163493, -5.520840484228896727 ) ) ;
#13814 = VECTOR ( 'NONE', #2331, 1000.000000000000000 ) ;
#13815 = ORIENTED_EDGE ( 'NONE', *, *, #11583, .T. ) ;
#13816 = ADVANCED_FACE ( 'NONE', ( #5339 ), #12867, .T. ) ;
#13817 = CARTESIAN_POINT ( 'NONE',  ( -12.99579180576516890, -11.31471392308272605, -1.551565153650648068E-15 ) ) ;
#13818 = ORIENTED_EDGE ( 'NONE', *, *, #13073, .T. ) ;
#13819 = LINE ( 'NONE', #888, #3227 ) ;
#13820 = CIRCLE ( 'NONE', #9983, 14.99999999999999112 ) ;
#13821 = CARTESIAN_POINT ( 'NONE',  ( 34.99999999999958789, 1.091249486606660213E-13, 2.500000000000000000 ) ) ;
#13822 = CARTESIAN_POINT ( 'NONE',  ( 10.35394582475457348, -71.99999999999978684, 3.762420212848049506 ) ) ;
#13823 = CARTESIAN_POINT ( 'NONE',  ( -0.1916457366473549029, -105.1818181818147764, -4.609965990740172437 ) ) ;
#13824 = CARTESIAN_POINT ( 'NONE',  ( 10.00000000000000711, 139.9999999999999716, -0.5000000000000000000 ) ) ;
#13825 = CYLINDRICAL_SURFACE ( 'NONE', #4863, 9.000000000008999024 ) ;
#13826 = AXIS2_PLACEMENT_3D ( 'NONE', #6895, #11181, #5858 ) ;
#13827 = DIRECTION ( 'NONE',  ( 1.000000000000000000, 0.000000000000000000, 0.000000000000000000 ) ) ;
#13828 = CYLINDRICAL_SURFACE ( 'NONE', #12973, 9.000000000008999024 ) ;
#13829 = AXIS2_PLACEMENT_3D ( 'NONE', #11399, #2851, #12609 ) ;
#13830 = ORIENTED_EDGE ( 'NONE', *, *, #12441, .F. ) ;
#13831 = EDGE_CURVE ( 'NONE', #11850, #11500, #3100, .T. ) ;
#13832 = EDGE_CURVE ( 'NONE', #1419, #7777, #13372, .T. ) ;
#13833 = CIRCLE ( 'NONE', #13147, 9.000000000008999024 ) ;
#13834 =( NAMED_UNIT ( * ) SI_UNIT ( $, .STERADIAN. ) SOLID_ANGLE_UNIT ( ) );
#13835 = ORIENTED_EDGE ( 'NONE', *, *, #11890, .T. ) ;
#13836 = EDGE_CURVE ( 'NONE', #9187, #6329, #810, .T. ) ;
#13837 = CARTESIAN_POINT ( 'NONE',  ( 15.29705854078140170, -19.91286587805129926, 1.949638918210574015E-15 ) ) ;
#13838 = CARTESIAN_POINT ( 'NONE',  ( -10.69346802281034847, 68.44840202376897764, -1.551312297200932909E-15 ) ) ;
#13839 = FACE_OUTER_BOUND ( 'NONE', #7954, .T. ) ;
#13840 = CARTESIAN_POINT ( 'NONE',  ( -10.09953664725343003, -70.24026703750095635, -0.01926284172907780090 ) ) ;
#13841 = CARTESIAN_POINT ( 'NONE',  ( -0.1430943862779323617, -159.4721208788122340, 1.503668078069826608 ) ) ;
#13842 = AXIS2_PLACEMENT_3D ( 'NONE', #1236, #5502, #187 ) ;
#13843 = LINE ( 'NONE', #6307, #8933 ) ;
#13844 = VERTEX_POINT ( 'NONE', #6330 ) ;
#13845 = VERTEX_POINT ( 'NONE', #2112 ) ;
#13846 = ADVANCED_FACE ( 'NONE', ( #6263 ), #1005, .T. ) ;
#13847 = CARTESIAN_POINT ( 'NONE',  ( -4.268720428656457067, 91.34229515271626099, -2.603909174561179540 ) ) ;
#13848 = CARTESIAN_POINT ( 'NONE',  ( 3.188279143310706054, -76.81818181818272251, 9.710576830322445119 ) ) ;
#13849 = ORIENTED_EDGE ( 'NONE', *, *, #4887, .T. ) ;
#13850 = ADVANCED_FACE ( 'NONE', ( #5274 ), #1822, .T. ) ;
#13851 = DIRECTION ( 'NONE',  ( -6.158143864569485777E-17, -2.736152283717910599E-16, 1.000000000000000000 ) ) ;
#13852 = EDGE_CURVE ( 'NONE', #1727, #2504, #8848, .T. ) ;
#13853 = FACE_OUTER_BOUND ( 'NONE', #6565, .T. ) ;
#13854 =( BOUNDED_SURFACE ( )  B_SPLINE_SURFACE ( 3, 3, ( 
 ( #2911, #9499, #7182, #5014 ),
 ( #4222, #9296, #5085, #3107 ),
 ( #8237, #3175, #9366, #11464 ),
 ( #7381, #5145, #1854, #6144 ) ),
 .UNSPECIFIED., .F., .F., .F. ) 
 B_SPLINE_SURFACE_WITH_KNOTS ( ( 4, 4 ),
 ( 4, 4 ),
 ( 0.000000000000000000, 1.000000000000000000 ),
 ( 0.000000000000000000, 1.000000000000000000 ),
 .UNSPECIFIED. ) 
 GEOMETRIC_REPRESENTATION_ITEM ( )  RATIONAL_B_SPLINE_SURFACE ( (
 ( 1.000000000000000000, 0.3333333333333334259, 0.3333333333333334259, 1.000000000000000000),
 ( 1.000000000000000000, 0.3333333333333334259, 0.3333333333333334259, 1.000000000000000000),
 ( 1.000000000000000000, 0.3333333333333334259, 0.3333333333333334259, 1.000000000000000000),
 ( 1.000000000000000000, 0.3333333333333334259, 0.3333333333333334259, 1.000000000000000000) ) ) 
 REPRESENTATION_ITEM ( '' )  SURFACE ( )  );
#13855 = CARTESIAN_POINT ( 'NONE',  ( -14.10210168181666113, -21.78333407367943053, 6.931746760319975387 ) ) ;
#13856 = CARTESIAN_POINT ( 'NONE',  ( 39.42692690461820604, 101.2627928944373679, -2.396630853396261251 ) ) ;
#13857 = DIRECTION ( 'NONE',  ( 0.000000000000000000, 0.000000000000000000, 1.000000000000000000 ) ) ;
#13858 = CARTESIAN_POINT ( 'NONE',  ( 2.869852970730162767, -107.6167546509799706, -6.080253893975354096 ) ) ;
#13859 = CARTESIAN_POINT ( 'NONE',  ( 35.20000000000001705, 106.3999999999999915, -0.5000000000000000000 ) ) ;
#13860 = ORIENTED_EDGE ( 'NONE', *, *, #12697, .F. ) ;
#13861 = ORIENTED_EDGE ( 'NONE', *, *, #13583, .F. ) ;
#13862 = EDGE_LOOP ( 'NONE', ( #9681, #167, #1892, #13170 ) ) ;
#13863 = ORIENTED_EDGE ( 'NONE', *, *, #6103, .T. ) ;
#13864 = CARTESIAN_POINT ( 'NONE',  ( 1.571852504498140624, -148.1710643681929866, -1.425705211460633670 ) ) ;
#13865 = EDGE_CURVE ( 'NONE', #13042, #13685, #9314, .T. ) ;
#13866 = CARTESIAN_POINT ( 'NONE',  ( -8.385254915620295790, 40.97916847270985130, -1.171624249618447227E-15 ) ) ;
#13867 = VERTEX_POINT ( 'NONE', #869 ) ;
#13868 = CARTESIAN_POINT ( 'NONE',  ( -10.69346802281034137, 40.17406817374067174, -21.38693604562068984 ) ) ;
#13869 = CARTESIAN_POINT ( 'NONE',  ( 8.374988411100524388, -92.13370500812025909, 2.112857200571143235 ) ) ;
#13870 = EDGE_CURVE ( 'NONE', #8314, #10021, #9750, .T. ) ;
#13871 = CARTESIAN_POINT ( 'NONE',  ( -0.05313321603431308410, -142.5800865801647319, -3.258060136337923129 ) ) ;
#13872 = DIRECTION ( 'NONE',  ( -0.6001121574638170753, 0.7999158696163758409, 1.850470399461381402E-16 ) ) ;
#13873 = CARTESIAN_POINT ( 'NONE',  ( -42.16244658108818300, 105.4500712252157655, 2.499999999999999556 ) ) ;
#13874 = CARTESIAN_POINT ( 'NONE',  ( -8.599520226296840875, -74.45454545454605011, -5.474475378420836869 ) ) ;
#13875 = CARTESIAN_POINT ( 'NONE',  ( 25.00000000000000355, 120.0000000000000142, -2.499999999999998668 ) ) ;
#13876 = DIRECTION ( 'NONE',  ( 1.000000000000000000, 3.469446951953615372E-15, 0.000000000000000000 ) ) ;
#13877 = CIRCLE ( 'NONE', #8918, 9.000000000008999024 ) ;
#13878 = FACE_OUTER_BOUND ( 'NONE', #7291, .T. ) ;
#13879 = VERTEX_POINT ( 'NONE', #4635 ) ;
#13880 = CARTESIAN_POINT ( 'NONE',  ( -2.224981447605033136, -153.6493506492698771, 4.266231359686146973 ) ) ;
#13881 = ORIENTED_EDGE ( 'NONE', *, *, #10211, .F. ) ;
#13882 = CARTESIAN_POINT ( 'NONE',  ( 12.99579180576516180, -11.31471392308272428, 25.99158361153033425 ) ) ;
#13883 = ORIENTED_EDGE ( 'NONE', *, *, #9972, .T. ) ;
#13884 = CARTESIAN_POINT ( 'NONE',  ( 0.000000000000000000, 71.01020514433645303, -0.5000000000000000000 ) ) ;
#13885 = DIRECTION ( 'NONE',  ( -1.000000000000000000, 0.000000000000000000, 0.000000000000000000 ) ) ;
#13886 = AXIS2_PLACEMENT_3D ( 'NONE', #1309, #4457, #6440 ) ;
#13887 = CARTESIAN_POINT ( 'NONE',  ( -6.296481028167455030, -65.63636363759458447, -1.027962039461249866 ) ) ;
#13888 = AXIS2_PLACEMENT_3D ( 'NONE', #2320, #2257, #10798 ) ;
#13889 = CARTESIAN_POINT ( 'NONE',  ( -18.54049621773915746, 27.07720798311999388, 7.500000000000000000 ) ) ;
#13890 = CARTESIAN_POINT ( 'NONE',  ( -10.69346802281033959, 11.89973432371241202, -21.38693604562068984 ) ) ;
#13891 = CARTESIAN_POINT ( 'NONE',  ( -10.00000000000000000, 92.00000000000000000, 0.5000000000000000000 ) ) ;
#13892 = DIRECTION ( 'NONE',  ( -6.158143864569485777E-17, -2.736152283717910599E-16, 1.000000000000000000 ) ) ;
#13893 = DIRECTION ( 'NONE',  ( -6.158143864569485777E-17, -2.736152283717910599E-16, 1.000000000000000000 ) ) ;
#13894 = CIRCLE ( 'NONE', #8476, 50.00000000000001421 ) ;
#13895 = ORIENTED_EDGE ( 'NONE', *, *, #13252, .F. ) ;
#13896 = FILL_AREA_STYLE_COLOUR ( '', #3720 ) ;
#13897 = ORIENTED_EDGE ( 'NONE', *, *, #5886, .T. ) ;
#13898 = CARTESIAN_POINT ( 'NONE',  ( -2.517691654963332357E-15, 90.00000000000000000, -1.589271161308885878E-16 ) ) ;
#13899 = NEXT_ASSEMBLY_USAGE_OCCURRENCE ( 'NAUO1', ' ', ' ', #9678, #3939, $ ) ;
#13900 = NEXT_ASSEMBLY_USAGE_OCCURRENCE ( 'NAUO2', ' ', ' ', #9678, #2214, $ ) ;
#13901 = NEXT_ASSEMBLY_USAGE_OCCURRENCE ( 'NAUO3', ' ', ' ', #9678, #8055, $ ) ;
#13902 = NEXT_ASSEMBLY_USAGE_OCCURRENCE ( 'NAUO4', ' ', ' ', #9678, #4712, $ ) ;
#13903 = NEXT_ASSEMBLY_USAGE_OCCURRENCE ( 'NAUO5', ' ', ' ', #9678, #11145, $ ) ;
#13904 = NEXT_ASSEMBLY_USAGE_OCCURRENCE ( 'NAUO6', ' ', ' ', #9678, #8055, $ ) ;
#13905 = NEXT_ASSEMBLY_USAGE_OCCURRENCE ( 'NAUO7', ' ', ' ', #9678, #11145, $ ) ;
ENDSEC;
END-ISO-10303-21;
